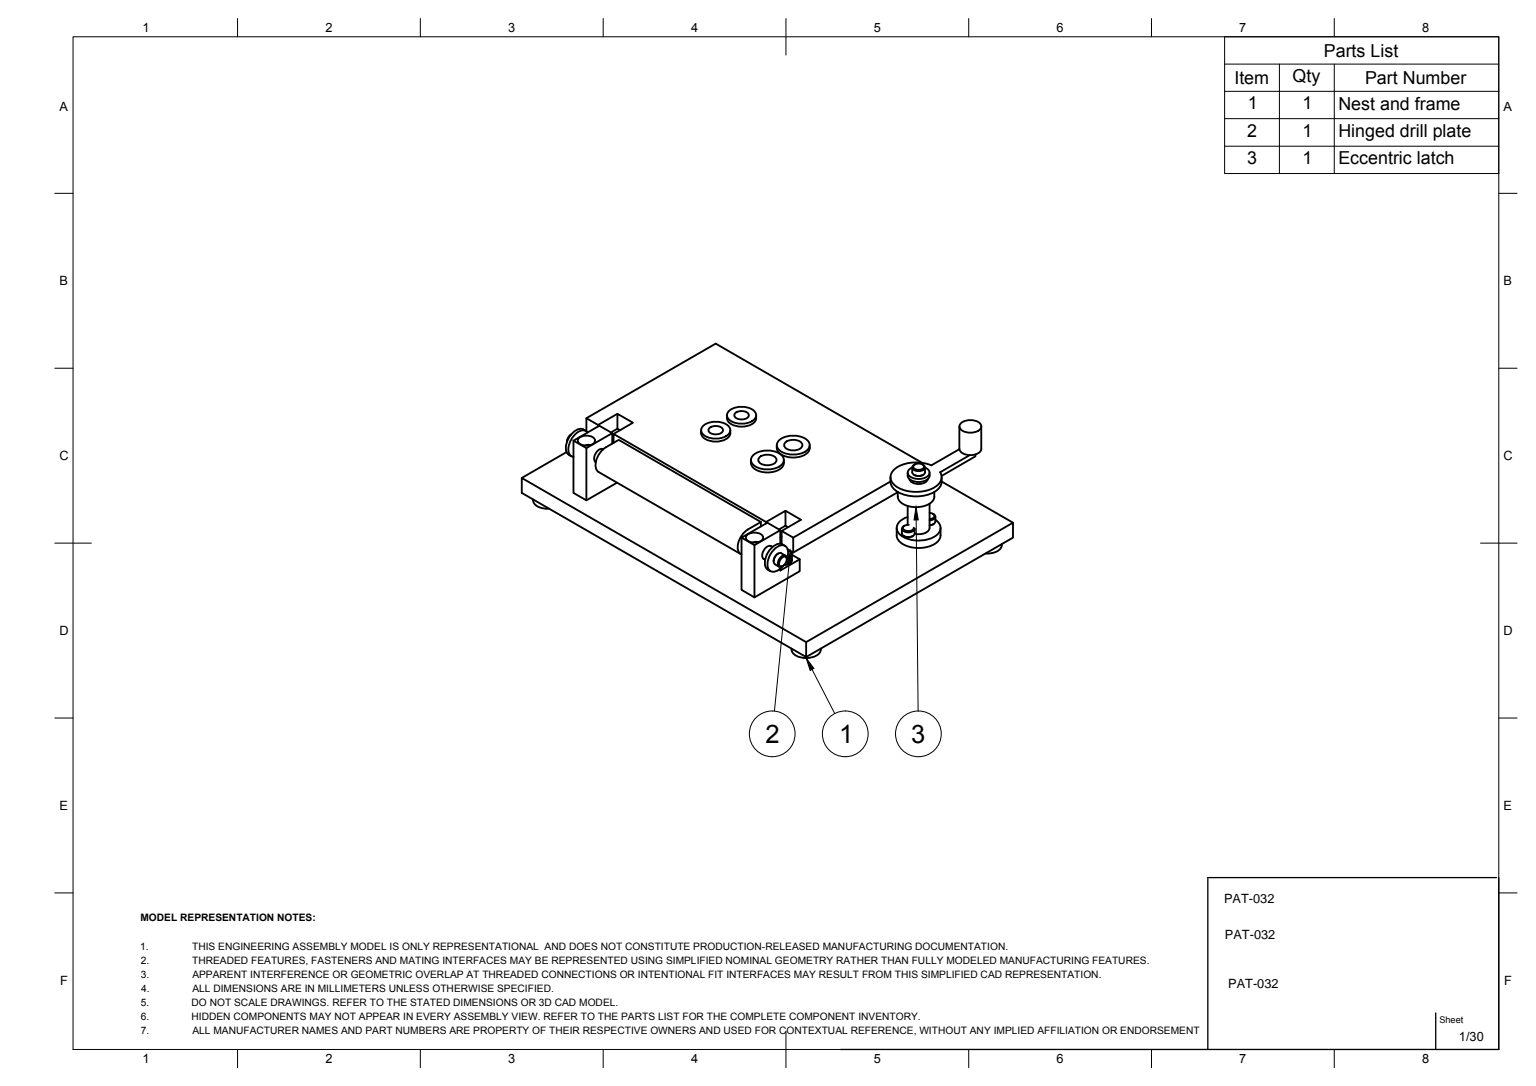
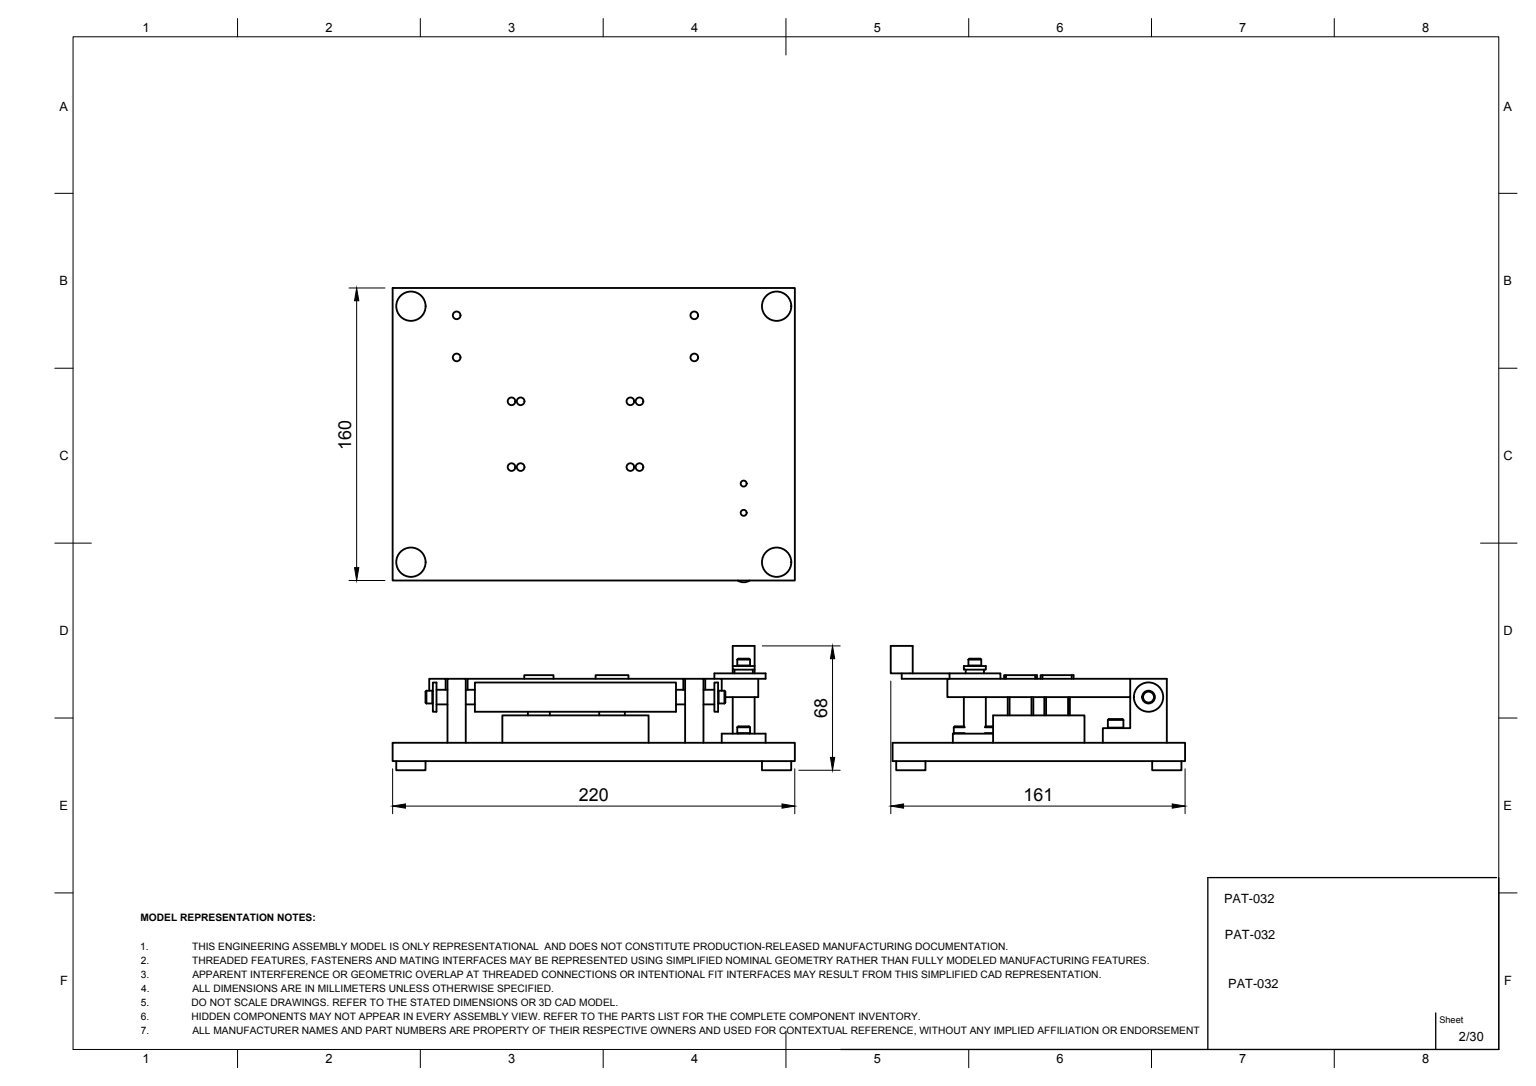
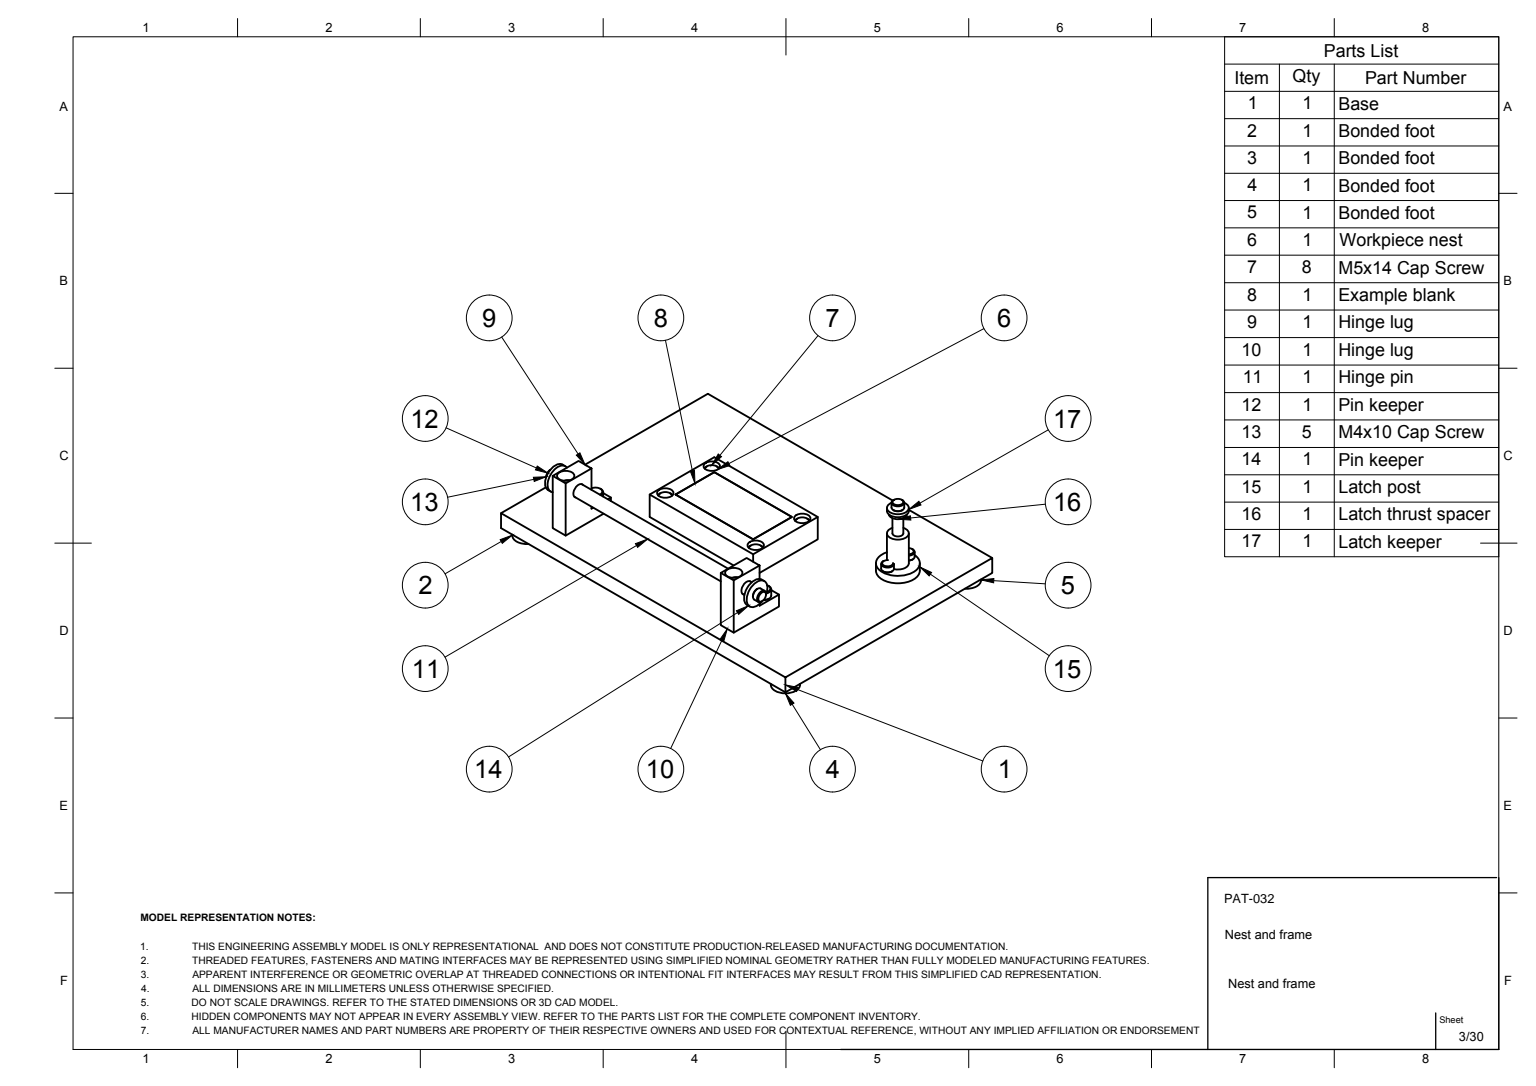
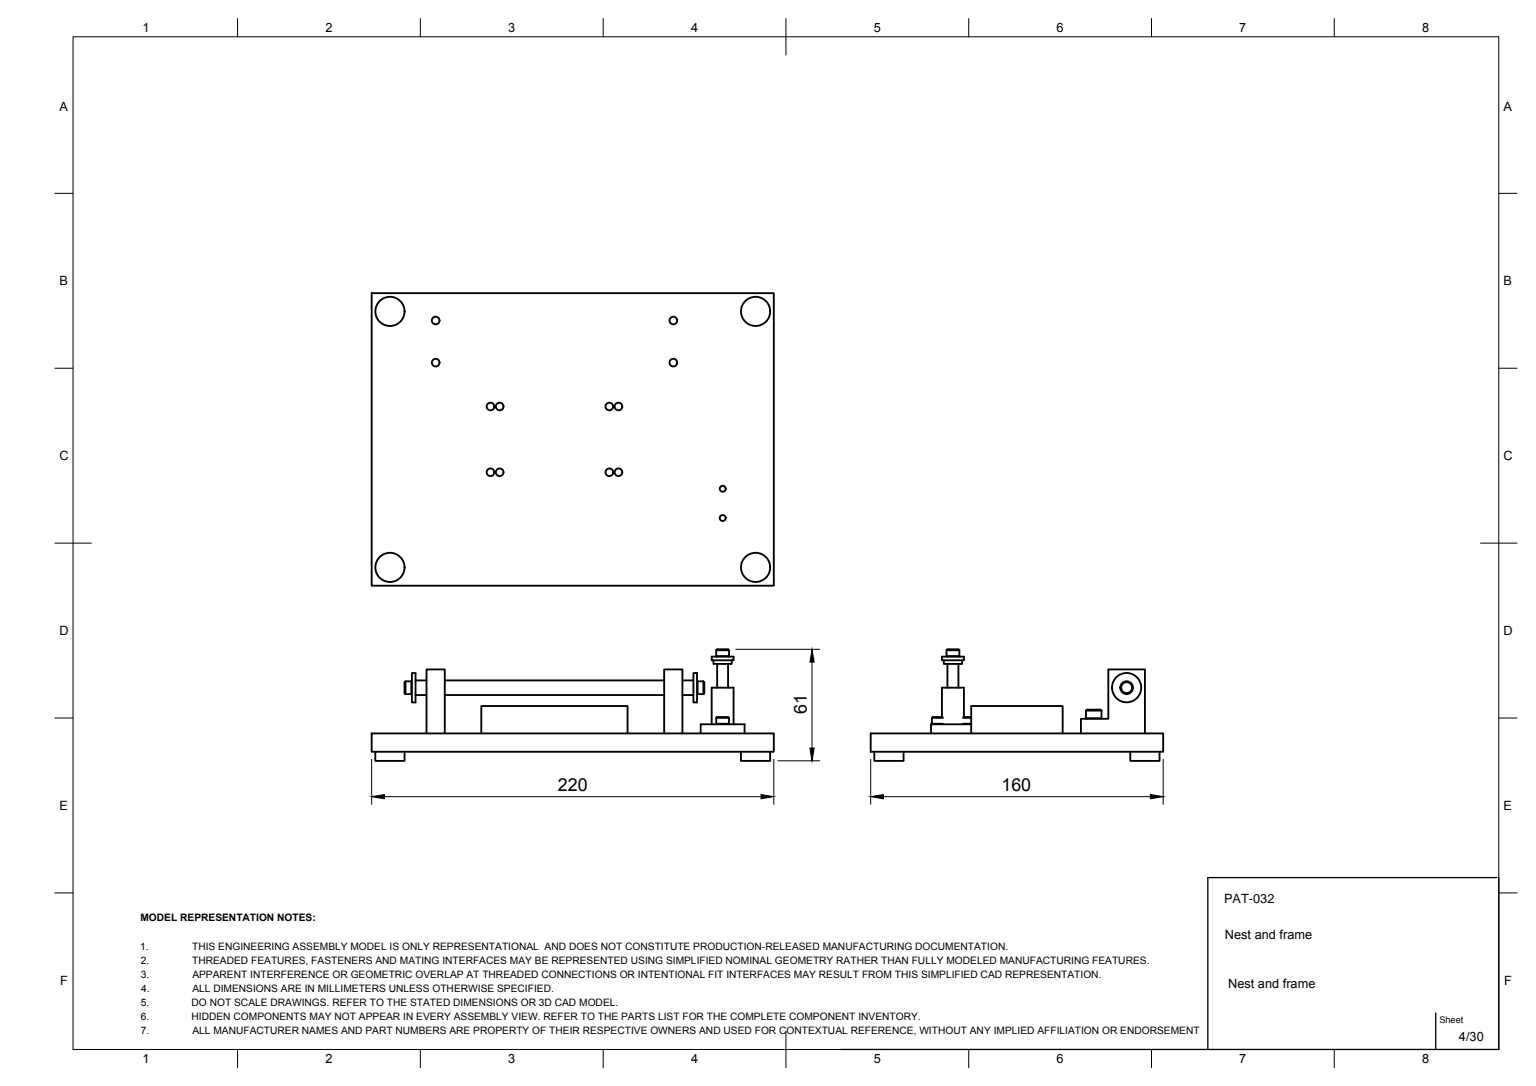
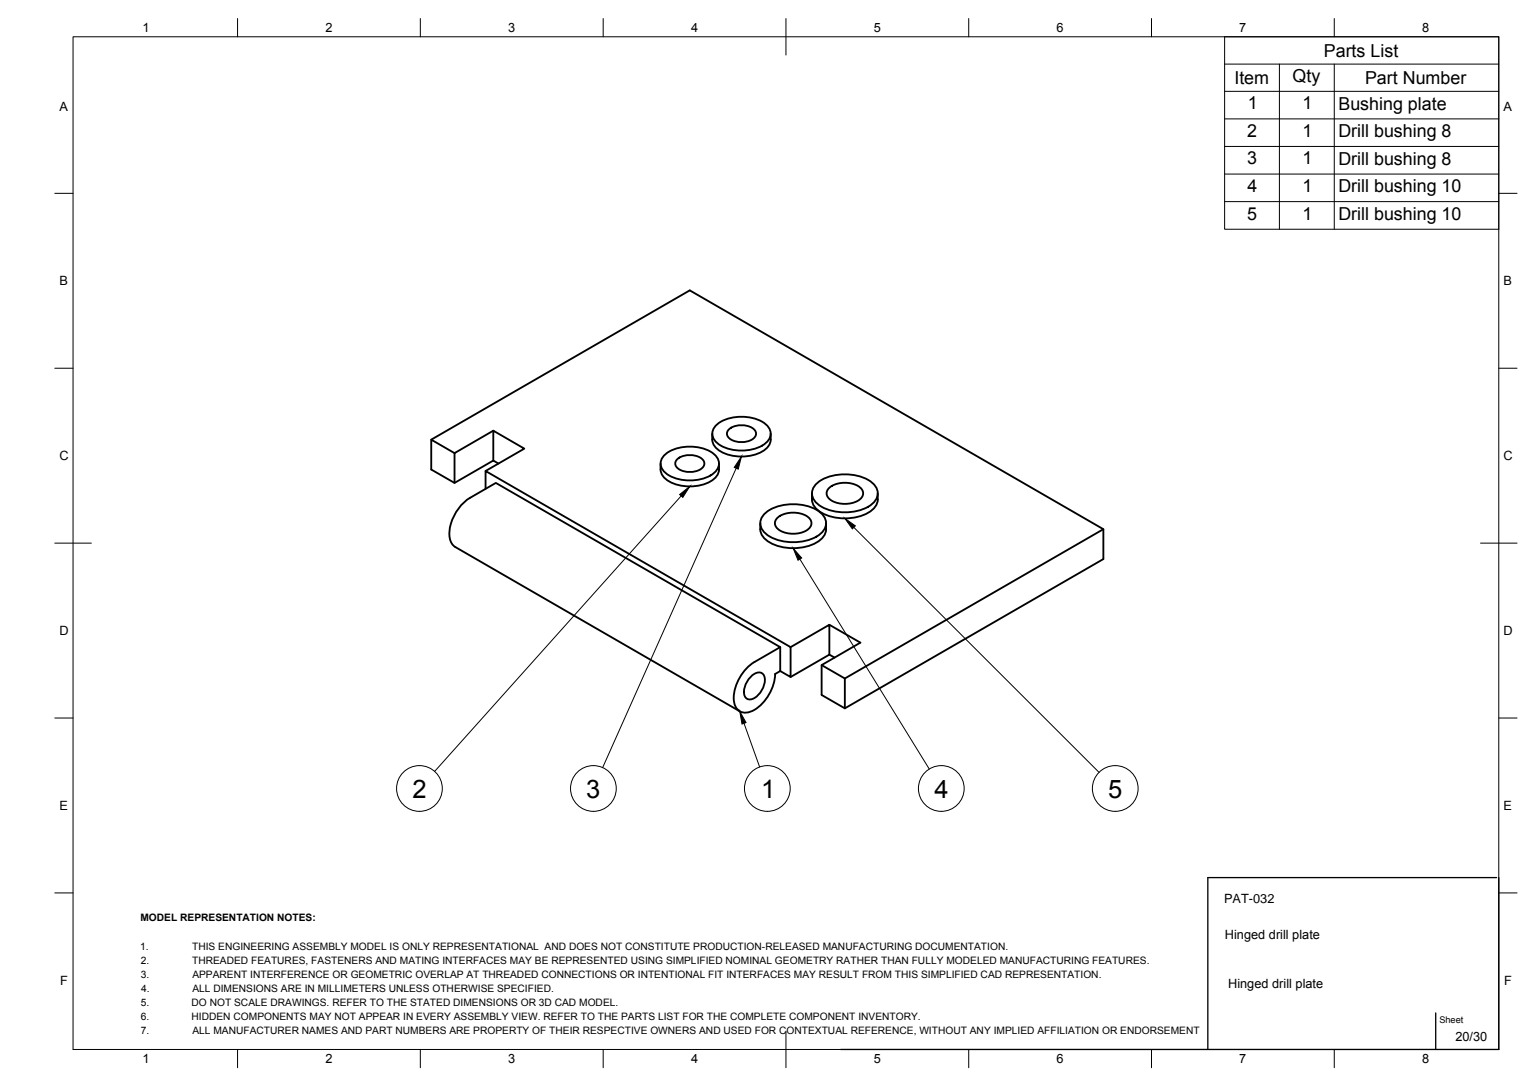
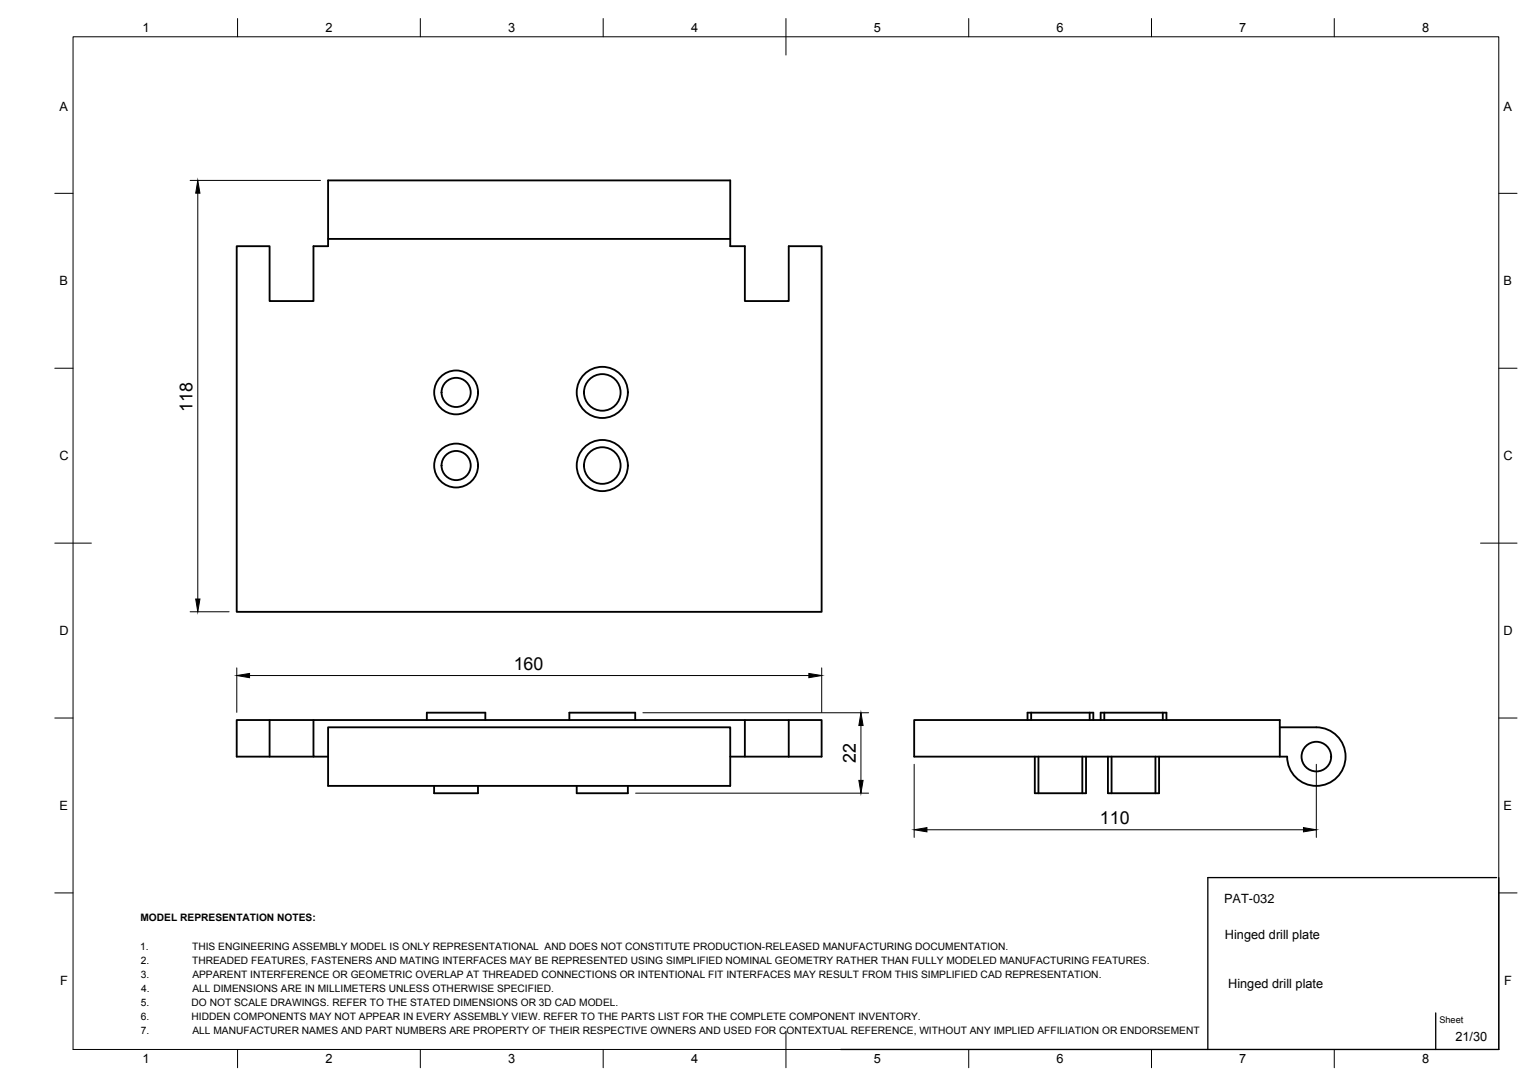
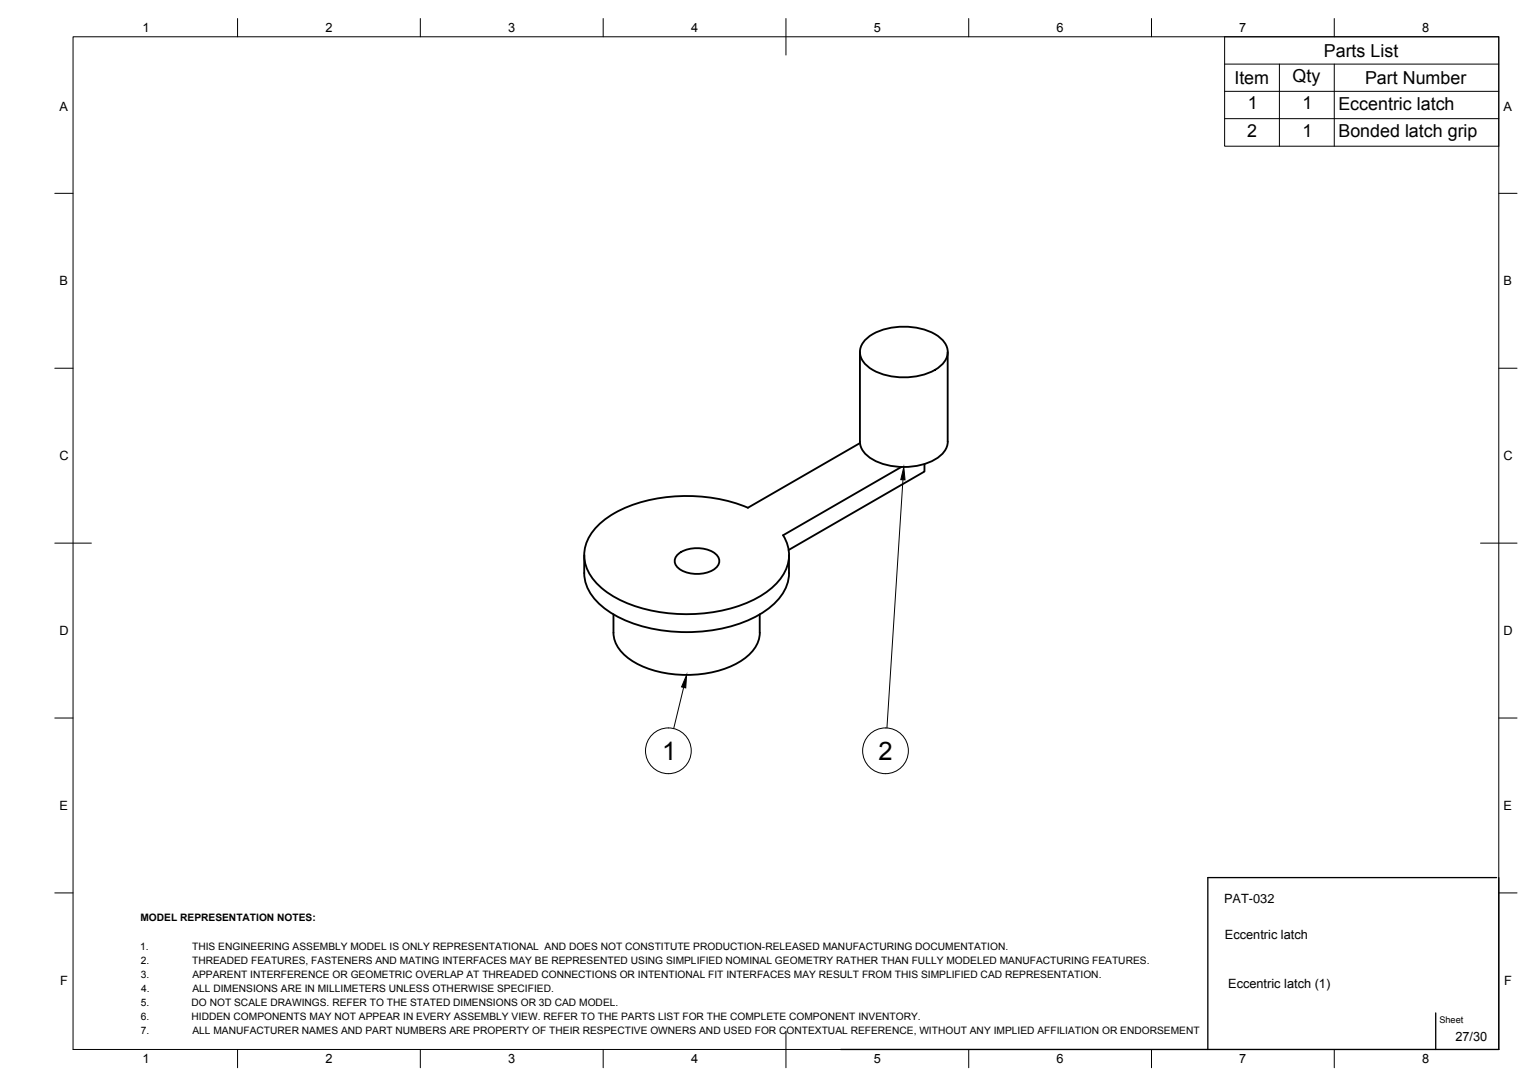
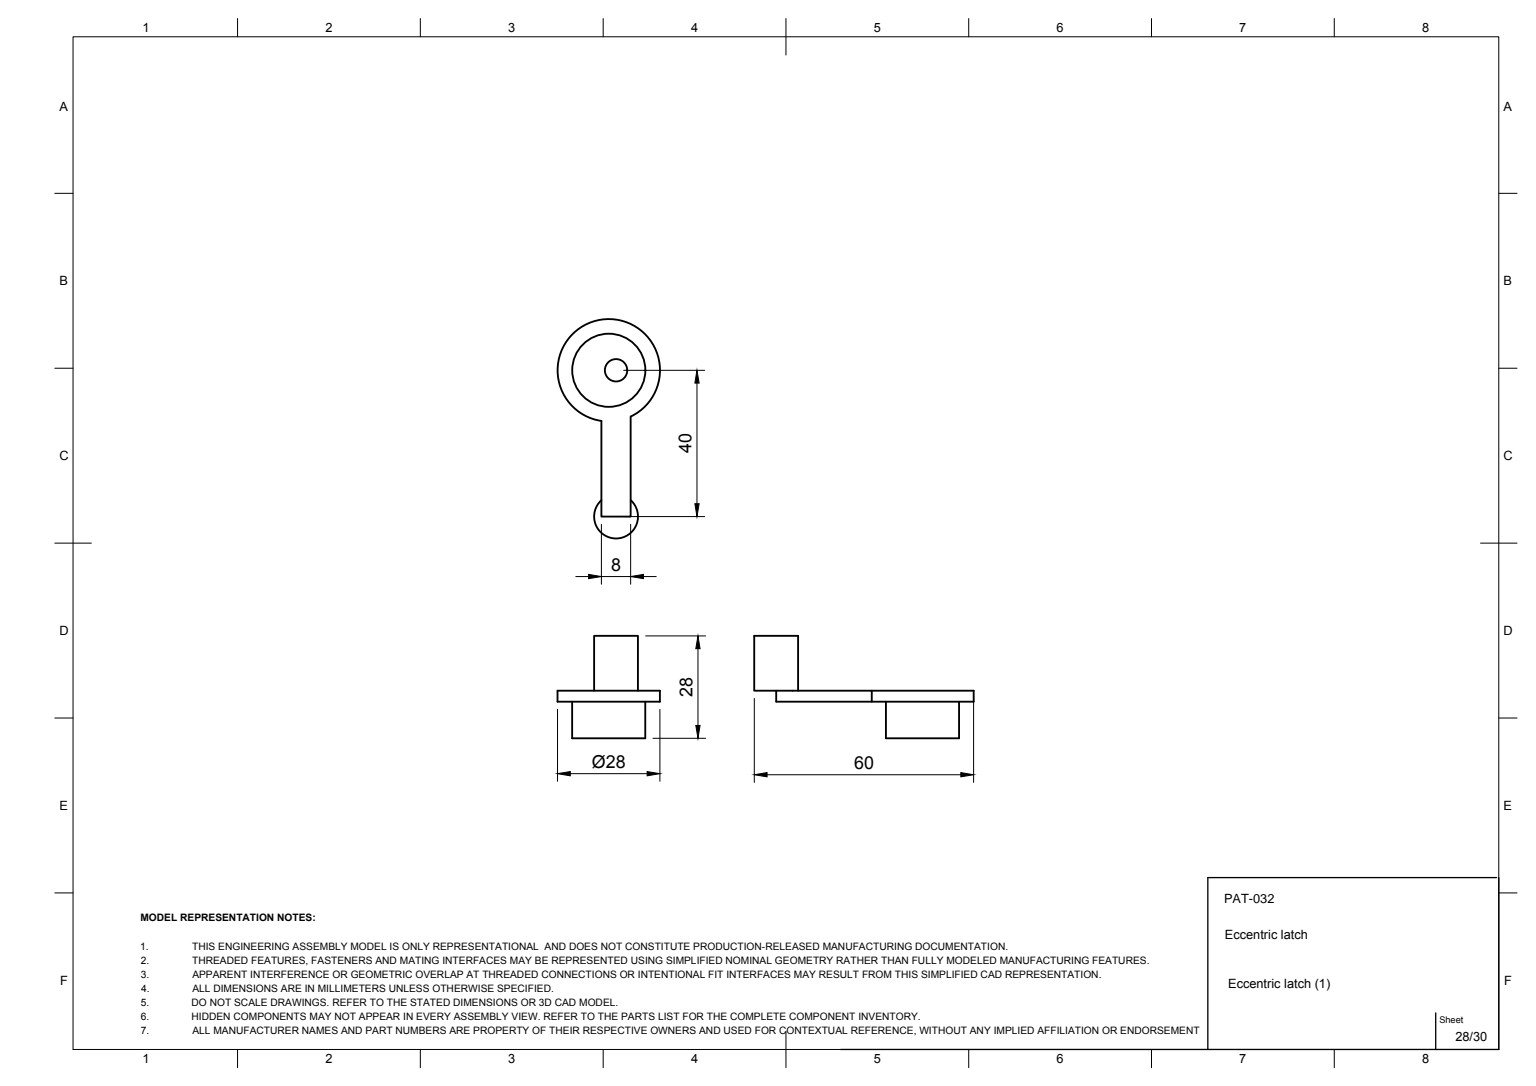
ISO-10303-21;
HEADER;
/* Generated by software containing ST-Developer
 * from STEP Tools, Inc. (www.steptools.com) 
 */

FILE_DESCRIPTION(
/* description */ ('Drill jig with bushing plate'),
/* implementation_level */ '2;1');

FILE_NAME(
/* name */ 'PAT-032',
/* time_stamp */ '2026-10-27T10:51:08-07:00',
/* author */ (''),
/* organization */ (''),
/* preprocessor_version */ 'ST-DEVELOPER v20.2',
/* originating_system */ 'Autodesk Translation Framework v15.17.0.0',
/* authorisation */ '');

FILE_SCHEMA (('AUTOMOTIVE_DESIGN { 1 0 10303 214 3 1 1 }'));
ENDSEC;

DATA;
#10=MECHANICAL_DESIGN_GEOMETRIC_PRESENTATION_REPRESENTATION('',(#223,#224,
#225,#226,#227,#228,#229,#230,#231,#232,#233,#234,#235,#236,#237,#238,#239,
#240,#241,#242,#243,#244,#245,#246),#6638);
#11=ITEM_DEFINED_TRANSFORMATION($,$,#3883,#4179);
#12=ITEM_DEFINED_TRANSFORMATION($,$,#3932,#4180);
#13=ITEM_DEFINED_TRANSFORMATION($,$,#3938,#4181);
#14=ITEM_DEFINED_TRANSFORMATION($,$,#3944,#4182);
#15=ITEM_DEFINED_TRANSFORMATION($,$,#3950,#4183);
#16=ITEM_DEFINED_TRANSFORMATION($,$,#3956,#4184);
#17=ITEM_DEFINED_TRANSFORMATION($,$,#3996,#4185);
#18=ITEM_DEFINED_TRANSFORMATION($,$,#4003,#4186);
#19=ITEM_DEFINED_TRANSFORMATION($,$,#4025,#4187);
#20=ITEM_DEFINED_TRANSFORMATION($,$,#4047,#4188);
#21=ITEM_DEFINED_TRANSFORMATION($,$,#4061,#4189);
#22=ITEM_DEFINED_TRANSFORMATION($,$,#4070,#4190);
#23=ITEM_DEFINED_TRANSFORMATION($,$,#4079,#4191);
#24=ITEM_DEFINED_TRANSFORMATION($,$,#4113,#4192);
#25=ITEM_DEFINED_TRANSFORMATION($,$,#4122,#4193);
#26=ITEM_DEFINED_TRANSFORMATION($,$,#4131,#4194);
#27=ITEM_DEFINED_TRANSFORMATION($,$,#4131,#4195);
#28=ITEM_DEFINED_TRANSFORMATION($,$,#4131,#4196);
#29=ITEM_DEFINED_TRANSFORMATION($,$,#4131,#4197);
#30=ITEM_DEFINED_TRANSFORMATION($,$,#4131,#4198);
#31=ITEM_DEFINED_TRANSFORMATION($,$,#4131,#4199);
#32=ITEM_DEFINED_TRANSFORMATION($,$,#4131,#4200);
#33=ITEM_DEFINED_TRANSFORMATION($,$,#4131,#4201);
#34=ITEM_DEFINED_TRANSFORMATION($,$,#4155,#4202);
#35=ITEM_DEFINED_TRANSFORMATION($,$,#4155,#4203);
#36=ITEM_DEFINED_TRANSFORMATION($,$,#4155,#4204);
#37=ITEM_DEFINED_TRANSFORMATION($,$,#4155,#4205);
#38=ITEM_DEFINED_TRANSFORMATION($,$,#4155,#4206);
#39=ITEM_DEFINED_TRANSFORMATION($,$,#4208,#4296);
#40=ITEM_DEFINED_TRANSFORMATION($,$,#4244,#4297);
#41=ITEM_DEFINED_TRANSFORMATION($,$,#4257,#4298);
#42=ITEM_DEFINED_TRANSFORMATION($,$,#4270,#4299);
#43=ITEM_DEFINED_TRANSFORMATION($,$,#4283,#4300);
#44=ITEM_DEFINED_TRANSFORMATION($,$,#4302,#4324);
#45=ITEM_DEFINED_TRANSFORMATION($,$,#4318,#4325);
#46=ITEM_DEFINED_TRANSFORMATION($,$,#3882,#4326);
#47=ITEM_DEFINED_TRANSFORMATION($,$,#4207,#4327);
#48=ITEM_DEFINED_TRANSFORMATION($,$,#4301,#4328);
#49=(
REPRESENTATION_RELATIONSHIP($,$,#6739,#6738)
REPRESENTATION_RELATIONSHIP_WITH_TRANSFORMATION(#11)
SHAPE_REPRESENTATION_RELATIONSHIP()
);
#50=(
REPRESENTATION_RELATIONSHIP($,$,#6740,#6738)
REPRESENTATION_RELATIONSHIP_WITH_TRANSFORMATION(#12)
SHAPE_REPRESENTATION_RELATIONSHIP()
);
#51=(
REPRESENTATION_RELATIONSHIP($,$,#6741,#6738)
REPRESENTATION_RELATIONSHIP_WITH_TRANSFORMATION(#13)
SHAPE_REPRESENTATION_RELATIONSHIP()
);
#52=(
REPRESENTATION_RELATIONSHIP($,$,#6742,#6738)
REPRESENTATION_RELATIONSHIP_WITH_TRANSFORMATION(#14)
SHAPE_REPRESENTATION_RELATIONSHIP()
);
#53=(
REPRESENTATION_RELATIONSHIP($,$,#6743,#6738)
REPRESENTATION_RELATIONSHIP_WITH_TRANSFORMATION(#15)
SHAPE_REPRESENTATION_RELATIONSHIP()
);
#54=(
REPRESENTATION_RELATIONSHIP($,$,#6744,#6738)
REPRESENTATION_RELATIONSHIP_WITH_TRANSFORMATION(#16)
SHAPE_REPRESENTATION_RELATIONSHIP()
);
#55=(
REPRESENTATION_RELATIONSHIP($,$,#6745,#6738)
REPRESENTATION_RELATIONSHIP_WITH_TRANSFORMATION(#17)
SHAPE_REPRESENTATION_RELATIONSHIP()
);
#56=(
REPRESENTATION_RELATIONSHIP($,$,#6746,#6738)
REPRESENTATION_RELATIONSHIP_WITH_TRANSFORMATION(#18)
SHAPE_REPRESENTATION_RELATIONSHIP()
);
#57=(
REPRESENTATION_RELATIONSHIP($,$,#6747,#6738)
REPRESENTATION_RELATIONSHIP_WITH_TRANSFORMATION(#19)
SHAPE_REPRESENTATION_RELATIONSHIP()
);
#58=(
REPRESENTATION_RELATIONSHIP($,$,#6748,#6738)
REPRESENTATION_RELATIONSHIP_WITH_TRANSFORMATION(#20)
SHAPE_REPRESENTATION_RELATIONSHIP()
);
#59=(
REPRESENTATION_RELATIONSHIP($,$,#6749,#6738)
REPRESENTATION_RELATIONSHIP_WITH_TRANSFORMATION(#21)
SHAPE_REPRESENTATION_RELATIONSHIP()
);
#60=(
REPRESENTATION_RELATIONSHIP($,$,#6750,#6738)
REPRESENTATION_RELATIONSHIP_WITH_TRANSFORMATION(#22)
SHAPE_REPRESENTATION_RELATIONSHIP()
);
#61=(
REPRESENTATION_RELATIONSHIP($,$,#6751,#6738)
REPRESENTATION_RELATIONSHIP_WITH_TRANSFORMATION(#23)
SHAPE_REPRESENTATION_RELATIONSHIP()
);
#62=(
REPRESENTATION_RELATIONSHIP($,$,#6752,#6738)
REPRESENTATION_RELATIONSHIP_WITH_TRANSFORMATION(#24)
SHAPE_REPRESENTATION_RELATIONSHIP()
);
#63=(
REPRESENTATION_RELATIONSHIP($,$,#6753,#6738)
REPRESENTATION_RELATIONSHIP_WITH_TRANSFORMATION(#25)
SHAPE_REPRESENTATION_RELATIONSHIP()
);
#64=(
REPRESENTATION_RELATIONSHIP($,$,#6754,#6738)
REPRESENTATION_RELATIONSHIP_WITH_TRANSFORMATION(#26)
SHAPE_REPRESENTATION_RELATIONSHIP()
);
#65=(
REPRESENTATION_RELATIONSHIP($,$,#6754,#6738)
REPRESENTATION_RELATIONSHIP_WITH_TRANSFORMATION(#27)
SHAPE_REPRESENTATION_RELATIONSHIP()
);
#66=(
REPRESENTATION_RELATIONSHIP($,$,#6754,#6738)
REPRESENTATION_RELATIONSHIP_WITH_TRANSFORMATION(#28)
SHAPE_REPRESENTATION_RELATIONSHIP()
);
#67=(
REPRESENTATION_RELATIONSHIP($,$,#6754,#6738)
REPRESENTATION_RELATIONSHIP_WITH_TRANSFORMATION(#29)
SHAPE_REPRESENTATION_RELATIONSHIP()
);
#68=(
REPRESENTATION_RELATIONSHIP($,$,#6754,#6738)
REPRESENTATION_RELATIONSHIP_WITH_TRANSFORMATION(#30)
SHAPE_REPRESENTATION_RELATIONSHIP()
);
#69=(
REPRESENTATION_RELATIONSHIP($,$,#6754,#6738)
REPRESENTATION_RELATIONSHIP_WITH_TRANSFORMATION(#31)
SHAPE_REPRESENTATION_RELATIONSHIP()
);
#70=(
REPRESENTATION_RELATIONSHIP($,$,#6754,#6738)
REPRESENTATION_RELATIONSHIP_WITH_TRANSFORMATION(#32)
SHAPE_REPRESENTATION_RELATIONSHIP()
);
#71=(
REPRESENTATION_RELATIONSHIP($,$,#6754,#6738)
REPRESENTATION_RELATIONSHIP_WITH_TRANSFORMATION(#33)
SHAPE_REPRESENTATION_RELATIONSHIP()
);
#72=(
REPRESENTATION_RELATIONSHIP($,$,#6755,#6738)
REPRESENTATION_RELATIONSHIP_WITH_TRANSFORMATION(#34)
SHAPE_REPRESENTATION_RELATIONSHIP()
);
#73=(
REPRESENTATION_RELATIONSHIP($,$,#6755,#6738)
REPRESENTATION_RELATIONSHIP_WITH_TRANSFORMATION(#35)
SHAPE_REPRESENTATION_RELATIONSHIP()
);
#74=(
REPRESENTATION_RELATIONSHIP($,$,#6755,#6738)
REPRESENTATION_RELATIONSHIP_WITH_TRANSFORMATION(#36)
SHAPE_REPRESENTATION_RELATIONSHIP()
);
#75=(
REPRESENTATION_RELATIONSHIP($,$,#6755,#6738)
REPRESENTATION_RELATIONSHIP_WITH_TRANSFORMATION(#37)
SHAPE_REPRESENTATION_RELATIONSHIP()
);
#76=(
REPRESENTATION_RELATIONSHIP($,$,#6755,#6738)
REPRESENTATION_RELATIONSHIP_WITH_TRANSFORMATION(#38)
SHAPE_REPRESENTATION_RELATIONSHIP()
);
#77=(
REPRESENTATION_RELATIONSHIP($,$,#6757,#6756)
REPRESENTATION_RELATIONSHIP_WITH_TRANSFORMATION(#39)
SHAPE_REPRESENTATION_RELATIONSHIP()
);
#78=(
REPRESENTATION_RELATIONSHIP($,$,#6758,#6756)
REPRESENTATION_RELATIONSHIP_WITH_TRANSFORMATION(#40)
SHAPE_REPRESENTATION_RELATIONSHIP()
);
#79=(
REPRESENTATION_RELATIONSHIP($,$,#6759,#6756)
REPRESENTATION_RELATIONSHIP_WITH_TRANSFORMATION(#41)
SHAPE_REPRESENTATION_RELATIONSHIP()
);
#80=(
REPRESENTATION_RELATIONSHIP($,$,#6760,#6756)
REPRESENTATION_RELATIONSHIP_WITH_TRANSFORMATION(#42)
SHAPE_REPRESENTATION_RELATIONSHIP()
);
#81=(
REPRESENTATION_RELATIONSHIP($,$,#6761,#6756)
REPRESENTATION_RELATIONSHIP_WITH_TRANSFORMATION(#43)
SHAPE_REPRESENTATION_RELATIONSHIP()
);
#82=(
REPRESENTATION_RELATIONSHIP($,$,#6763,#6762)
REPRESENTATION_RELATIONSHIP_WITH_TRANSFORMATION(#44)
SHAPE_REPRESENTATION_RELATIONSHIP()
);
#83=(
REPRESENTATION_RELATIONSHIP($,$,#6764,#6762)
REPRESENTATION_RELATIONSHIP_WITH_TRANSFORMATION(#45)
SHAPE_REPRESENTATION_RELATIONSHIP()
);
#84=(
REPRESENTATION_RELATIONSHIP($,$,#6738,#6737)
REPRESENTATION_RELATIONSHIP_WITH_TRANSFORMATION(#46)
SHAPE_REPRESENTATION_RELATIONSHIP()
);
#85=(
REPRESENTATION_RELATIONSHIP($,$,#6756,#6737)
REPRESENTATION_RELATIONSHIP_WITH_TRANSFORMATION(#47)
SHAPE_REPRESENTATION_RELATIONSHIP()
);
#86=(
REPRESENTATION_RELATIONSHIP($,$,#6762,#6737)
REPRESENTATION_RELATIONSHIP_WITH_TRANSFORMATION(#48)
SHAPE_REPRESENTATION_RELATIONSHIP()
);
#87=CONTEXT_DEPENDENT_SHAPE_REPRESENTATION(#49,#6690);
#88=CONTEXT_DEPENDENT_SHAPE_REPRESENTATION(#50,#6691);
#89=CONTEXT_DEPENDENT_SHAPE_REPRESENTATION(#51,#6692);
#90=CONTEXT_DEPENDENT_SHAPE_REPRESENTATION(#52,#6693);
#91=CONTEXT_DEPENDENT_SHAPE_REPRESENTATION(#53,#6694);
#92=CONTEXT_DEPENDENT_SHAPE_REPRESENTATION(#54,#6695);
#93=CONTEXT_DEPENDENT_SHAPE_REPRESENTATION(#55,#6696);
#94=CONTEXT_DEPENDENT_SHAPE_REPRESENTATION(#56,#6697);
#95=CONTEXT_DEPENDENT_SHAPE_REPRESENTATION(#57,#6698);
#96=CONTEXT_DEPENDENT_SHAPE_REPRESENTATION(#58,#6699);
#97=CONTEXT_DEPENDENT_SHAPE_REPRESENTATION(#59,#6700);
#98=CONTEXT_DEPENDENT_SHAPE_REPRESENTATION(#60,#6701);
#99=CONTEXT_DEPENDENT_SHAPE_REPRESENTATION(#61,#6702);
#100=CONTEXT_DEPENDENT_SHAPE_REPRESENTATION(#62,#6703);
#101=CONTEXT_DEPENDENT_SHAPE_REPRESENTATION(#63,#6704);
#102=CONTEXT_DEPENDENT_SHAPE_REPRESENTATION(#64,#6705);
#103=CONTEXT_DEPENDENT_SHAPE_REPRESENTATION(#65,#6706);
#104=CONTEXT_DEPENDENT_SHAPE_REPRESENTATION(#66,#6707);
#105=CONTEXT_DEPENDENT_SHAPE_REPRESENTATION(#67,#6708);
#106=CONTEXT_DEPENDENT_SHAPE_REPRESENTATION(#68,#6709);
#107=CONTEXT_DEPENDENT_SHAPE_REPRESENTATION(#69,#6710);
#108=CONTEXT_DEPENDENT_SHAPE_REPRESENTATION(#70,#6711);
#109=CONTEXT_DEPENDENT_SHAPE_REPRESENTATION(#71,#6712);
#110=CONTEXT_DEPENDENT_SHAPE_REPRESENTATION(#72,#6713);
#111=CONTEXT_DEPENDENT_SHAPE_REPRESENTATION(#73,#6714);
#112=CONTEXT_DEPENDENT_SHAPE_REPRESENTATION(#74,#6715);
#113=CONTEXT_DEPENDENT_SHAPE_REPRESENTATION(#75,#6716);
#114=CONTEXT_DEPENDENT_SHAPE_REPRESENTATION(#76,#6717);
#115=CONTEXT_DEPENDENT_SHAPE_REPRESENTATION(#77,#6724);
#116=CONTEXT_DEPENDENT_SHAPE_REPRESENTATION(#78,#6725);
#117=CONTEXT_DEPENDENT_SHAPE_REPRESENTATION(#79,#6726);
#118=CONTEXT_DEPENDENT_SHAPE_REPRESENTATION(#80,#6727);
#119=CONTEXT_DEPENDENT_SHAPE_REPRESENTATION(#81,#6728);
#120=CONTEXT_DEPENDENT_SHAPE_REPRESENTATION(#82,#6732);
#121=CONTEXT_DEPENDENT_SHAPE_REPRESENTATION(#83,#6733);
#122=CONTEXT_DEPENDENT_SHAPE_REPRESENTATION(#84,#6734);
#123=CONTEXT_DEPENDENT_SHAPE_REPRESENTATION(#85,#6735);
#124=CONTEXT_DEPENDENT_SHAPE_REPRESENTATION(#86,#6736);
#125=NEXT_ASSEMBLY_USAGE_OCCURRENCE('Base:1','Base:1','Base:1',#6767,#6768,
'Base:1');
#126=NEXT_ASSEMBLY_USAGE_OCCURRENCE('Bonded foot:1','Bonded foot:1',
'Bonded foot:1',#6767,#6769,'Bonded foot:1');
#127=NEXT_ASSEMBLY_USAGE_OCCURRENCE('Bonded foot (1):1',
'Bonded foot (1):1','Bonded foot (1):1',#6767,#6770,'Bonded foot (1):1');
#128=NEXT_ASSEMBLY_USAGE_OCCURRENCE('Bonded foot (2):1',
'Bonded foot (2):1','Bonded foot (2):1',#6767,#6771,'Bonded foot (2):1');
#129=NEXT_ASSEMBLY_USAGE_OCCURRENCE('Bonded foot (3):1',
'Bonded foot (3):1','Bonded foot (3):1',#6767,#6772,'Bonded foot (3):1');
#130=NEXT_ASSEMBLY_USAGE_OCCURRENCE('Workpiece nest:1',
'Workpiece nest:1','Workpiece nest:1',#6767,#6773,'Workpiece nest:1');
#131=NEXT_ASSEMBLY_USAGE_OCCURRENCE('Example blank:1','Example blank:1',
'Example blank:1',#6767,#6774,'Example blank:1');
#132=NEXT_ASSEMBLY_USAGE_OCCURRENCE('Hinge lug:1','Hinge lug:1',
'Hinge lug:1',#6767,#6775,'Hinge lug:1');
#133=NEXT_ASSEMBLY_USAGE_OCCURRENCE('Hinge lug (1):1','Hinge lug (1):1',
'Hinge lug (1):1',#6767,#6776,'Hinge lug (1):1');
#134=NEXT_ASSEMBLY_USAGE_OCCURRENCE('Hinge pin:1','Hinge pin:1',
'Hinge pin:1',#6767,#6777,'Hinge pin:1');
#135=NEXT_ASSEMBLY_USAGE_OCCURRENCE('Pin keeper:1','Pin keeper:1',
'Pin keeper:1',#6767,#6778,'Pin keeper:1');
#136=NEXT_ASSEMBLY_USAGE_OCCURRENCE('Pin keeper (1):1',
'Pin keeper (1):1','Pin keeper (1):1',#6767,#6779,'Pin keeper (1):1');
#137=NEXT_ASSEMBLY_USAGE_OCCURRENCE('Latch post:1','Latch post:1',
'Latch post:1',#6767,#6780,'Latch post:1');
#138=NEXT_ASSEMBLY_USAGE_OCCURRENCE('Latch thrust spacer:1',
'Latch thrust spacer:1','Latch thrust spacer:1',#6767,#6781,
'Latch thrust spacer:1');
#139=NEXT_ASSEMBLY_USAGE_OCCURRENCE('Latch keeper:1','Latch keeper:1',
'Latch keeper:1',#6767,#6782,'Latch keeper:1');
#140=NEXT_ASSEMBLY_USAGE_OCCURRENCE('M5x14 Cap Screw:2',
'M5x14 Cap Screw:2','M5x14 Cap Screw:2',#6767,#6783,'M5x14 Cap Screw:2');
#141=NEXT_ASSEMBLY_USAGE_OCCURRENCE('M5x14 Cap Screw:3',
'M5x14 Cap Screw:3','M5x14 Cap Screw:3',#6767,#6783,'M5x14 Cap Screw:3');
#142=NEXT_ASSEMBLY_USAGE_OCCURRENCE('M5x14 Cap Screw:4',
'M5x14 Cap Screw:4','M5x14 Cap Screw:4',#6767,#6783,'M5x14 Cap Screw:4');
#143=NEXT_ASSEMBLY_USAGE_OCCURRENCE('M5x14 Cap Screw:5',
'M5x14 Cap Screw:5','M5x14 Cap Screw:5',#6767,#6783,'M5x14 Cap Screw:5');
#144=NEXT_ASSEMBLY_USAGE_OCCURRENCE('M5x14 Cap Screw:6',
'M5x14 Cap Screw:6','M5x14 Cap Screw:6',#6767,#6783,'M5x14 Cap Screw:6');
#145=NEXT_ASSEMBLY_USAGE_OCCURRENCE('M5x14 Cap Screw:7',
'M5x14 Cap Screw:7','M5x14 Cap Screw:7',#6767,#6783,'M5x14 Cap Screw:7');
#146=NEXT_ASSEMBLY_USAGE_OCCURRENCE('M5x14 Cap Screw:8',
'M5x14 Cap Screw:8','M5x14 Cap Screw:8',#6767,#6783,'M5x14 Cap Screw:8');
#147=NEXT_ASSEMBLY_USAGE_OCCURRENCE('M5x14 Cap Screw:9',
'M5x14 Cap Screw:9','M5x14 Cap Screw:9',#6767,#6783,'M5x14 Cap Screw:9');
#148=NEXT_ASSEMBLY_USAGE_OCCURRENCE('M4x10 Cap Screw:2',
'M4x10 Cap Screw:2','M4x10 Cap Screw:2',#6767,#6784,'M4x10 Cap Screw:2');
#149=NEXT_ASSEMBLY_USAGE_OCCURRENCE('M4x10 Cap Screw:3',
'M4x10 Cap Screw:3','M4x10 Cap Screw:3',#6767,#6784,'M4x10 Cap Screw:3');
#150=NEXT_ASSEMBLY_USAGE_OCCURRENCE('M4x10 Cap Screw:4',
'M4x10 Cap Screw:4','M4x10 Cap Screw:4',#6767,#6784,'M4x10 Cap Screw:4');
#151=NEXT_ASSEMBLY_USAGE_OCCURRENCE('M4x10 Cap Screw:5',
'M4x10 Cap Screw:5','M4x10 Cap Screw:5',#6767,#6784,'M4x10 Cap Screw:5');
#152=NEXT_ASSEMBLY_USAGE_OCCURRENCE('M4x10 Cap Screw:6',
'M4x10 Cap Screw:6','M4x10 Cap Screw:6',#6767,#6784,'M4x10 Cap Screw:6');
#153=NEXT_ASSEMBLY_USAGE_OCCURRENCE('Bushing plate:1','Bushing plate:1',
'Bushing plate:1',#6785,#6786,'Bushing plate:1');
#154=NEXT_ASSEMBLY_USAGE_OCCURRENCE('Drill bushing 8:1',
'Drill bushing 8:1','Drill bushing 8:1',#6785,#6787,'Drill bushing 8:1');
#155=NEXT_ASSEMBLY_USAGE_OCCURRENCE('Drill bushing 8 (1):1',
'Drill bushing 8 (1):1','Drill bushing 8 (1):1',#6785,#6788,
'Drill bushing 8 (1):1');
#156=NEXT_ASSEMBLY_USAGE_OCCURRENCE('Drill bushing 10:1',
'Drill bushing 10:1','Drill bushing 10:1',#6785,#6789,
'Drill bushing 10:1');
#157=NEXT_ASSEMBLY_USAGE_OCCURRENCE('Drill bushing 10 (1):1',
'Drill bushing 10 (1):1','Drill bushing 10 (1):1',#6785,#6790,
'Drill bushing 10 (1):1');
#158=NEXT_ASSEMBLY_USAGE_OCCURRENCE('Eccentric latch:1',
'Eccentric latch:1','Eccentric latch:1',#6791,#6792,'Eccentric latch:1');
#159=NEXT_ASSEMBLY_USAGE_OCCURRENCE('Bonded latch grip:1',
'Bonded latch grip:1','Bonded latch grip:1',#6791,#6793,
'Bonded latch grip:1');
#160=NEXT_ASSEMBLY_USAGE_OCCURRENCE('Nest and frame:1',
'Nest and frame:1','Nest and frame:1',#6766,#6767,'Nest and frame:1');
#161=NEXT_ASSEMBLY_USAGE_OCCURRENCE('Hinged drill plate:1',
'Hinged drill plate:1','Hinged drill plate:1',#6766,#6785,
'Hinged drill plate:1');
#162=NEXT_ASSEMBLY_USAGE_OCCURRENCE('Eccentric latch (1):1',
'Eccentric latch (1):1','Eccentric latch (1):1',#6766,#6791,
'Eccentric latch (1):1');
#163=CONICAL_SURFACE('',#4144,0.4,0.785398163397448);
#164=CONICAL_SURFACE('',#4148,0.41,0.785398163397448);
#165=CONICAL_SURFACE('',#4152,0.26,0.463647609000806);
#166=CONICAL_SURFACE('',#4168,0.325,0.785398163397448);
#167=CONICAL_SURFACE('',#4172,0.335,0.785398163397448);
#168=CONICAL_SURFACE('',#4176,0.21,0.463647609000806);
#169=ORIENTED_CLOSED_SHELL('',*,#3605,.F.);
#170=ORIENTED_CLOSED_SHELL('',*,#3607,.F.);
#171=BREP_WITH_VOIDS('Body1',#3606,(#169));
#172=BREP_WITH_VOIDS('Body1',#3608,(#170));
#173=B_SPLINE_CURVE_WITH_KNOTS('',3,(#5774,#5775,#5776,#5777,#5778,#5779,
#5780,#5781,#5782,#5783,#5784,#5785,#5786,#5787,#5788,#5789,#5790,#5791,
#5792,#5793,#5794,#5795,#5796,#5797,#5798,#5799,#5800,#5801,#5802,#5803,
#5804,#5805,#5806,#5807,#5808,#5809,#5810,#5811,#5812,#5813,#5814,#5815,
#5816,#5817,#5818,#5819,#5820,#5821,#5822,#5823),.UNSPECIFIED.,.T.,.F.,
(4,2,2,2,2,2,2,2,2,2,2,2,2,2,2,2,2,2,2,2,2,2,2,2,4),(0.,0.177519856988816,
0.355039713977633,0.436196019741432,0.517352325505232,0.678532215702782,
0.839712105900332,1.00089199609788,1.16207188629543,1.24322819205923,1.32438449782303,
1.50190435481185,1.67942421180066,1.85694406878948,2.0344639257783,2.1156202315421,
2.1967765373059,2.35795642750345,2.519136317701,2.68031620789855,2.8414960980961,
2.9226524038599,3.0038087096237,3.18132856661251,3.35884842360133),
 .UNSPECIFIED.);
#174=B_SPLINE_CURVE_WITH_KNOTS('',3,(#5889,#5890,#5891,#5892,#5893,#5894,
#5895,#5896,#5897,#5898,#5899,#5900,#5901,#5902,#5903,#5904,#5905,#5906,
#5907,#5908,#5909,#5910,#5911,#5912,#5913,#5914,#5915,#5916,#5917,#5918,
#5919,#5920,#5921,#5922,#5923,#5924,#5925,#5926,#5927,#5928,#5929,#5930,
#5931,#5932,#5933,#5934,#5935,#5936,#5937,#5938),.UNSPECIFIED.,.T.,.F.,
(4,2,2,2,2,2,2,2,2,2,2,2,2,2,2,2,2,2,2,2,2,2,2,2,4),(0.,0.177519856988816,
0.355039713977633,0.436196019741432,0.517352325505232,0.678532215702782,
0.839712105900332,1.00089199609788,1.16207188629543,1.24322819205923,1.32438449782303,
1.50190435481185,1.67942421180066,1.85694406878948,2.0344639257783,2.1156202315421,
2.1967765373059,2.35795642750345,2.519136317701,2.68031620789855,2.8414960980961,
2.9226524038599,3.0038087096237,3.18132856661251,3.35884842360133),
 .UNSPECIFIED.);
#175=SHAPE_REPRESENTATION_RELATIONSHIP('SRR','None',#6739,#199);
#176=SHAPE_REPRESENTATION_RELATIONSHIP('SRR','None',#6740,#200);
#177=SHAPE_REPRESENTATION_RELATIONSHIP('SRR','None',#6741,#201);
#178=SHAPE_REPRESENTATION_RELATIONSHIP('SRR','None',#6742,#202);
#179=SHAPE_REPRESENTATION_RELATIONSHIP('SRR','None',#6743,#203);
#180=SHAPE_REPRESENTATION_RELATIONSHIP('SRR','None',#6744,#204);
#181=SHAPE_REPRESENTATION_RELATIONSHIP('SRR','None',#6745,#205);
#182=SHAPE_REPRESENTATION_RELATIONSHIP('SRR','None',#6746,#206);
#183=SHAPE_REPRESENTATION_RELATIONSHIP('SRR','None',#6747,#207);
#184=SHAPE_REPRESENTATION_RELATIONSHIP('SRR','None',#6748,#208);
#185=SHAPE_REPRESENTATION_RELATIONSHIP('SRR','None',#6749,#209);
#186=SHAPE_REPRESENTATION_RELATIONSHIP('SRR','None',#6750,#210);
#187=SHAPE_REPRESENTATION_RELATIONSHIP('SRR','None',#6751,#211);
#188=SHAPE_REPRESENTATION_RELATIONSHIP('SRR','None',#6752,#212);
#189=SHAPE_REPRESENTATION_RELATIONSHIP('SRR','None',#6753,#213);
#190=SHAPE_REPRESENTATION_RELATIONSHIP('SRR','None',#6754,#214);
#191=SHAPE_REPRESENTATION_RELATIONSHIP('SRR','None',#6755,#215);
#192=SHAPE_REPRESENTATION_RELATIONSHIP('SRR','None',#6757,#216);
#193=SHAPE_REPRESENTATION_RELATIONSHIP('SRR','None',#6758,#217);
#194=SHAPE_REPRESENTATION_RELATIONSHIP('SRR','None',#6759,#218);
#195=SHAPE_REPRESENTATION_RELATIONSHIP('SRR','None',#6760,#219);
#196=SHAPE_REPRESENTATION_RELATIONSHIP('SRR','None',#6761,#220);
#197=SHAPE_REPRESENTATION_RELATIONSHIP('SRR','None',#6763,#221);
#198=SHAPE_REPRESENTATION_RELATIONSHIP('SRR','None',#6764,#222);
#199=ADVANCED_BREP_SHAPE_REPRESENTATION('',(#247),#6612);
#200=ADVANCED_BREP_SHAPE_REPRESENTATION('',(#248),#6613);
#201=ADVANCED_BREP_SHAPE_REPRESENTATION('',(#249),#6614);
#202=ADVANCED_BREP_SHAPE_REPRESENTATION('',(#250),#6615);
#203=ADVANCED_BREP_SHAPE_REPRESENTATION('',(#251),#6616);
#204=ADVANCED_BREP_SHAPE_REPRESENTATION('',(#252),#6617);
#205=ADVANCED_BREP_SHAPE_REPRESENTATION('',(#253),#6618);
#206=ADVANCED_BREP_SHAPE_REPRESENTATION('',(#254),#6619);
#207=ADVANCED_BREP_SHAPE_REPRESENTATION('',(#255),#6620);
#208=ADVANCED_BREP_SHAPE_REPRESENTATION('',(#256),#6621);
#209=ADVANCED_BREP_SHAPE_REPRESENTATION('',(#257),#6622);
#210=ADVANCED_BREP_SHAPE_REPRESENTATION('',(#258),#6623);
#211=ADVANCED_BREP_SHAPE_REPRESENTATION('',(#259),#6624);
#212=ADVANCED_BREP_SHAPE_REPRESENTATION('',(#260),#6625);
#213=ADVANCED_BREP_SHAPE_REPRESENTATION('',(#261),#6626);
#214=ADVANCED_BREP_SHAPE_REPRESENTATION('',(#171),#6627);
#215=ADVANCED_BREP_SHAPE_REPRESENTATION('',(#172),#6628);
#216=ADVANCED_BREP_SHAPE_REPRESENTATION('',(#262),#6630);
#217=ADVANCED_BREP_SHAPE_REPRESENTATION('',(#263),#6631);
#218=ADVANCED_BREP_SHAPE_REPRESENTATION('',(#264),#6632);
#219=ADVANCED_BREP_SHAPE_REPRESENTATION('',(#265),#6633);
#220=ADVANCED_BREP_SHAPE_REPRESENTATION('',(#266),#6634);
#221=ADVANCED_BREP_SHAPE_REPRESENTATION('',(#267),#6636);
#222=ADVANCED_BREP_SHAPE_REPRESENTATION('',(#268),#6637);
#223=STYLED_ITEM('',(#6922),#247);
#224=STYLED_ITEM('',(#6957),#248);
#225=STYLED_ITEM('',(#6957),#249);
#226=STYLED_ITEM('',(#6957),#250);
#227=STYLED_ITEM('',(#6957),#251);
#228=STYLED_ITEM('',(#6936),#252);
#229=STYLED_ITEM('',(#6929),#253);
#230=STYLED_ITEM('',(#6957),#254);
#231=STYLED_ITEM('',(#6957),#255);
#232=STYLED_ITEM('',(#6943),#256);
#233=STYLED_ITEM('',(#6943),#257);
#234=STYLED_ITEM('',(#6943),#258);
#235=STYLED_ITEM('',(#6957),#259);
#236=STYLED_ITEM('',(#6936),#260);
#237=STYLED_ITEM('',(#6936),#261);
#238=STYLED_ITEM('',(#6950),#171);
#239=STYLED_ITEM('',(#6950),#172);
#240=STYLED_ITEM('',(#6957),#262);
#241=STYLED_ITEM('',(#6957),#263);
#242=STYLED_ITEM('',(#6957),#264);
#243=STYLED_ITEM('',(#6929),#265);
#244=STYLED_ITEM('',(#6929),#266);
#245=STYLED_ITEM('',(#6936),#267);
#246=STYLED_ITEM('',(#6950),#268);
#247=MANIFOLD_SOLID_BREP('Body1',#3590);
#248=MANIFOLD_SOLID_BREP('Body1',#3591);
#249=MANIFOLD_SOLID_BREP('Body1',#3592);
#250=MANIFOLD_SOLID_BREP('Body1',#3593);
#251=MANIFOLD_SOLID_BREP('Body1',#3594);
#252=MANIFOLD_SOLID_BREP('Body1',#3595);
#253=MANIFOLD_SOLID_BREP('Body1',#3596);
#254=MANIFOLD_SOLID_BREP('Body1',#3597);
#255=MANIFOLD_SOLID_BREP('Body1',#3598);
#256=MANIFOLD_SOLID_BREP('Body1',#3599);
#257=MANIFOLD_SOLID_BREP('Body1',#3600);
#258=MANIFOLD_SOLID_BREP('Body1',#3601);
#259=MANIFOLD_SOLID_BREP('Body1',#3602);
#260=MANIFOLD_SOLID_BREP('Body1',#3603);
#261=MANIFOLD_SOLID_BREP('Body1',#3604);
#262=MANIFOLD_SOLID_BREP('Body1',#3609);
#263=MANIFOLD_SOLID_BREP('Body1',#3610);
#264=MANIFOLD_SOLID_BREP('Body1',#3611);
#265=MANIFOLD_SOLID_BREP('Body1',#3612);
#266=MANIFOLD_SOLID_BREP('Body1',#3613);
#267=MANIFOLD_SOLID_BREP('Body1',#3614);
#268=MANIFOLD_SOLID_BREP('Body1',#3615);
#269=FACE_BOUND('',#734,.T.);
#270=FACE_BOUND('',#735,.T.);
#271=FACE_BOUND('',#736,.T.);
#272=FACE_BOUND('',#737,.T.);
#273=FACE_BOUND('',#738,.T.);
#274=FACE_BOUND('',#739,.T.);
#275=FACE_BOUND('',#740,.T.);
#276=FACE_BOUND('',#741,.T.);
#277=FACE_BOUND('',#742,.T.);
#278=FACE_BOUND('',#743,.T.);
#279=FACE_BOUND('',#744,.T.);
#280=FACE_BOUND('',#745,.T.);
#281=FACE_BOUND('',#746,.T.);
#282=FACE_BOUND('',#747,.T.);
#283=FACE_BOUND('',#749,.T.);
#284=FACE_BOUND('',#750,.T.);
#285=FACE_BOUND('',#751,.T.);
#286=FACE_BOUND('',#752,.T.);
#287=FACE_BOUND('',#753,.T.);
#288=FACE_BOUND('',#754,.T.);
#289=FACE_BOUND('',#755,.T.);
#290=FACE_BOUND('',#756,.T.);
#291=FACE_BOUND('',#757,.T.);
#292=FACE_BOUND('',#758,.T.);
#293=FACE_BOUND('',#759,.T.);
#294=FACE_BOUND('',#760,.T.);
#295=FACE_BOUND('',#761,.T.);
#296=FACE_BOUND('',#762,.T.);
#297=FACE_BOUND('',#777,.T.);
#298=FACE_BOUND('',#780,.T.);
#299=FACE_BOUND('',#783,.T.);
#300=FACE_BOUND('',#786,.T.);
#301=FACE_BOUND('',#801,.T.);
#302=FACE_BOUND('',#802,.T.);
#303=FACE_BOUND('',#803,.T.);
#304=FACE_BOUND('',#804,.T.);
#305=FACE_BOUND('',#805,.T.);
#306=FACE_BOUND('',#807,.T.);
#307=FACE_BOUND('',#808,.T.);
#308=FACE_BOUND('',#809,.T.);
#309=FACE_BOUND('',#810,.T.);
#310=FACE_BOUND('',#818,.T.);
#311=FACE_BOUND('',#820,.T.);
#312=FACE_BOUND('',#824,.T.);
#313=FACE_BOUND('',#826,.T.);
#314=FACE_BOUND('',#829,.T.);
#315=FACE_BOUND('',#832,.T.);
#316=FACE_BOUND('',#833,.T.);
#317=FACE_BOUND('',#836,.T.);
#318=FACE_BOUND('',#838,.T.);
#319=FACE_BOUND('',#840,.T.);
#320=FACE_BOUND('',#842,.T.);
#321=FACE_BOUND('',#846,.T.);
#322=FACE_BOUND('',#848,.T.);
#323=FACE_BOUND('',#851,.T.);
#324=FACE_BOUND('',#854,.T.);
#325=FACE_BOUND('',#855,.T.);
#326=FACE_BOUND('',#858,.T.);
#327=FACE_BOUND('',#860,.T.);
#328=FACE_BOUND('',#867,.T.);
#329=FACE_BOUND('',#869,.T.);
#330=FACE_BOUND('',#873,.T.);
#331=FACE_BOUND('',#875,.T.);
#332=FACE_BOUND('',#879,.T.);
#333=FACE_BOUND('',#881,.T.);
#334=FACE_BOUND('',#890,.T.);
#335=FACE_BOUND('',#894,.T.);
#336=FACE_BOUND('',#896,.T.);
#337=FACE_BOUND('',#898,.T.);
#338=FACE_BOUND('',#899,.T.);
#339=FACE_BOUND('',#903,.T.);
#340=FACE_BOUND('',#905,.T.);
#341=FACE_BOUND('',#909,.T.);
#342=FACE_BOUND('',#911,.T.);
#343=FACE_BOUND('',#926,.T.);
#344=FACE_BOUND('',#943,.T.);
#345=FACE_BOUND('',#951,.T.);
#346=FACE_BOUND('',#954,.T.);
#347=FACE_BOUND('',#962,.T.);
#348=FACE_BOUND('',#963,.T.);
#349=FACE_BOUND('',#964,.T.);
#350=FACE_BOUND('',#965,.T.);
#351=FACE_BOUND('',#975,.T.);
#352=FACE_BOUND('',#976,.T.);
#353=FACE_BOUND('',#977,.T.);
#354=FACE_BOUND('',#978,.T.);
#355=FACE_BOUND('',#980,.T.);
#356=FACE_BOUND('',#983,.T.);
#357=FACE_BOUND('',#987,.T.);
#358=FACE_BOUND('',#989,.T.);
#359=FACE_BOUND('',#992,.T.);
#360=FACE_BOUND('',#996,.T.);
#361=FACE_BOUND('',#998,.T.);
#362=FACE_BOUND('',#1001,.T.);
#363=FACE_BOUND('',#1005,.T.);
#364=FACE_BOUND('',#1007,.T.);
#365=FACE_BOUND('',#1010,.T.);
#366=FACE_BOUND('',#1014,.T.);
#367=FACE_BOUND('',#1020,.T.);
#368=FACE_BOUND('',#1022,.T.);
#369=FACE_BOUND('',#1026,.T.);
#370=PLANE('',#3926);
#371=PLANE('',#3927);
#372=PLANE('',#3928);
#373=PLANE('',#3929);
#374=PLANE('',#3930);
#375=PLANE('',#3931);
#376=PLANE('',#3936);
#377=PLANE('',#3937);
#378=PLANE('',#3942);
#379=PLANE('',#3943);
#380=PLANE('',#3948);
#381=PLANE('',#3949);
#382=PLANE('',#3954);
#383=PLANE('',#3955);
#384=PLANE('',#3960);
#385=PLANE('',#3965);
#386=PLANE('',#3970);
#387=PLANE('',#3975);
#388=PLANE('',#3985);
#389=PLANE('',#3986);
#390=PLANE('',#3987);
#391=PLANE('',#3988);
#392=PLANE('',#3989);
#393=PLANE('',#3990);
#394=PLANE('',#3991);
#395=PLANE('',#3992);
#396=PLANE('',#3993);
#397=PLANE('',#3994);
#398=PLANE('',#3995);
#399=PLANE('',#3997);
#400=PLANE('',#3998);
#401=PLANE('',#3999);
#402=PLANE('',#4000);
#403=PLANE('',#4001);
#404=PLANE('',#4002);
#405=PLANE('',#4007);
#406=PLANE('',#4017);
#407=PLANE('',#4018);
#408=PLANE('',#4019);
#409=PLANE('',#4020);
#410=PLANE('',#4021);
#411=PLANE('',#4022);
#412=PLANE('',#4023);
#413=PLANE('',#4024);
#414=PLANE('',#4029);
#415=PLANE('',#4039);
#416=PLANE('',#4040);
#417=PLANE('',#4041);
#418=PLANE('',#4042);
#419=PLANE('',#4043);
#420=PLANE('',#4044);
#421=PLANE('',#4045);
#422=PLANE('',#4046);
#423=PLANE('',#4051);
#424=PLANE('',#4055);
#425=PLANE('',#4059);
#426=PLANE('',#4060);
#427=PLANE('',#4068);
#428=PLANE('',#4069);
#429=PLANE('',#4077);
#430=PLANE('',#4078);
#431=PLANE('',#4083);
#432=PLANE('',#4084);
#433=PLANE('',#4091);
#434=PLANE('',#4103);
#435=PLANE('',#4110);
#436=PLANE('',#4111);
#437=PLANE('',#4112);
#438=PLANE('',#4120);
#439=PLANE('',#4121);
#440=PLANE('',#4129);
#441=PLANE('',#4130);
#442=PLANE('',#4132);
#443=PLANE('',#4133);
#444=PLANE('',#4134);
#445=PLANE('',#4135);
#446=PLANE('',#4136);
#447=PLANE('',#4137);
#448=PLANE('',#4138);
#449=PLANE('',#4139);
#450=PLANE('',#4140);
#451=PLANE('',#4142);
#452=PLANE('',#4150);
#453=PLANE('',#4156);
#454=PLANE('',#4157);
#455=PLANE('',#4158);
#456=PLANE('',#4159);
#457=PLANE('',#4160);
#458=PLANE('',#4161);
#459=PLANE('',#4162);
#460=PLANE('',#4163);
#461=PLANE('',#4164);
#462=PLANE('',#4166);
#463=PLANE('',#4174);
#464=PLANE('',#4221);
#465=PLANE('',#4224);
#466=PLANE('',#4225);
#467=PLANE('',#4230);
#468=PLANE('',#4231);
#469=PLANE('',#4232);
#470=PLANE('',#4233);
#471=PLANE('',#4234);
#472=PLANE('',#4235);
#473=PLANE('',#4236);
#474=PLANE('',#4237);
#475=PLANE('',#4238);
#476=PLANE('',#4239);
#477=PLANE('',#4240);
#478=PLANE('',#4241);
#479=PLANE('',#4242);
#480=PLANE('',#4243);
#481=PLANE('',#4245);
#482=PLANE('',#4250);
#483=PLANE('',#4256);
#484=PLANE('',#4258);
#485=PLANE('',#4263);
#486=PLANE('',#4269);
#487=PLANE('',#4271);
#488=PLANE('',#4276);
#489=PLANE('',#4282);
#490=PLANE('',#4284);
#491=PLANE('',#4289);
#492=PLANE('',#4295);
#493=PLANE('',#4306);
#494=PLANE('',#4307);
#495=PLANE('',#4308);
#496=PLANE('',#4309);
#497=PLANE('',#4311);
#498=PLANE('',#4317);
#499=PLANE('',#4322);
#500=PLANE('',#4323);
#501=FACE_OUTER_BOUND('',#715,.T.);
#502=FACE_OUTER_BOUND('',#716,.T.);
#503=FACE_OUTER_BOUND('',#717,.T.);
#504=FACE_OUTER_BOUND('',#718,.T.);
#505=FACE_OUTER_BOUND('',#719,.T.);
#506=FACE_OUTER_BOUND('',#720,.T.);
#507=FACE_OUTER_BOUND('',#721,.T.);
#508=FACE_OUTER_BOUND('',#722,.T.);
#509=FACE_OUTER_BOUND('',#723,.T.);
#510=FACE_OUTER_BOUND('',#724,.T.);
#511=FACE_OUTER_BOUND('',#725,.T.);
#512=FACE_OUTER_BOUND('',#726,.T.);
#513=FACE_OUTER_BOUND('',#727,.T.);
#514=FACE_OUTER_BOUND('',#728,.T.);
#515=FACE_OUTER_BOUND('',#729,.T.);
#516=FACE_OUTER_BOUND('',#730,.T.);
#517=FACE_OUTER_BOUND('',#731,.T.);
#518=FACE_OUTER_BOUND('',#732,.T.);
#519=FACE_OUTER_BOUND('',#733,.T.);
#520=FACE_OUTER_BOUND('',#748,.T.);
#521=FACE_OUTER_BOUND('',#763,.T.);
#522=FACE_OUTER_BOUND('',#764,.T.);
#523=FACE_OUTER_BOUND('',#765,.T.);
#524=FACE_OUTER_BOUND('',#766,.T.);
#525=FACE_OUTER_BOUND('',#767,.T.);
#526=FACE_OUTER_BOUND('',#768,.T.);
#527=FACE_OUTER_BOUND('',#769,.T.);
#528=FACE_OUTER_BOUND('',#770,.T.);
#529=FACE_OUTER_BOUND('',#771,.T.);
#530=FACE_OUTER_BOUND('',#772,.T.);
#531=FACE_OUTER_BOUND('',#773,.T.);
#532=FACE_OUTER_BOUND('',#774,.T.);
#533=FACE_OUTER_BOUND('',#775,.T.);
#534=FACE_OUTER_BOUND('',#776,.T.);
#535=FACE_OUTER_BOUND('',#778,.T.);
#536=FACE_OUTER_BOUND('',#779,.T.);
#537=FACE_OUTER_BOUND('',#781,.T.);
#538=FACE_OUTER_BOUND('',#782,.T.);
#539=FACE_OUTER_BOUND('',#784,.T.);
#540=FACE_OUTER_BOUND('',#785,.T.);
#541=FACE_OUTER_BOUND('',#787,.T.);
#542=FACE_OUTER_BOUND('',#788,.T.);
#543=FACE_OUTER_BOUND('',#789,.T.);
#544=FACE_OUTER_BOUND('',#790,.T.);
#545=FACE_OUTER_BOUND('',#791,.T.);
#546=FACE_OUTER_BOUND('',#792,.T.);
#547=FACE_OUTER_BOUND('',#793,.T.);
#548=FACE_OUTER_BOUND('',#794,.T.);
#549=FACE_OUTER_BOUND('',#795,.T.);
#550=FACE_OUTER_BOUND('',#796,.T.);
#551=FACE_OUTER_BOUND('',#797,.T.);
#552=FACE_OUTER_BOUND('',#798,.T.);
#553=FACE_OUTER_BOUND('',#799,.T.);
#554=FACE_OUTER_BOUND('',#800,.T.);
#555=FACE_OUTER_BOUND('',#806,.T.);
#556=FACE_OUTER_BOUND('',#811,.T.);
#557=FACE_OUTER_BOUND('',#812,.T.);
#558=FACE_OUTER_BOUND('',#813,.T.);
#559=FACE_OUTER_BOUND('',#814,.T.);
#560=FACE_OUTER_BOUND('',#815,.T.);
#561=FACE_OUTER_BOUND('',#816,.T.);
#562=FACE_OUTER_BOUND('',#817,.T.);
#563=FACE_OUTER_BOUND('',#819,.T.);
#564=FACE_OUTER_BOUND('',#821,.T.);
#565=FACE_OUTER_BOUND('',#822,.T.);
#566=FACE_OUTER_BOUND('',#823,.T.);
#567=FACE_OUTER_BOUND('',#825,.T.);
#568=FACE_OUTER_BOUND('',#827,.T.);
#569=FACE_OUTER_BOUND('',#828,.T.);
#570=FACE_OUTER_BOUND('',#830,.T.);
#571=FACE_OUTER_BOUND('',#831,.T.);
#572=FACE_OUTER_BOUND('',#834,.T.);
#573=FACE_OUTER_BOUND('',#835,.T.);
#574=FACE_OUTER_BOUND('',#837,.T.);
#575=FACE_OUTER_BOUND('',#839,.T.);
#576=FACE_OUTER_BOUND('',#841,.T.);
#577=FACE_OUTER_BOUND('',#843,.T.);
#578=FACE_OUTER_BOUND('',#844,.T.);
#579=FACE_OUTER_BOUND('',#845,.T.);
#580=FACE_OUTER_BOUND('',#847,.T.);
#581=FACE_OUTER_BOUND('',#849,.T.);
#582=FACE_OUTER_BOUND('',#850,.T.);
#583=FACE_OUTER_BOUND('',#852,.T.);
#584=FACE_OUTER_BOUND('',#853,.T.);
#585=FACE_OUTER_BOUND('',#856,.T.);
#586=FACE_OUTER_BOUND('',#857,.T.);
#587=FACE_OUTER_BOUND('',#859,.T.);
#588=FACE_OUTER_BOUND('',#861,.T.);
#589=FACE_OUTER_BOUND('',#862,.T.);
#590=FACE_OUTER_BOUND('',#863,.T.);
#591=FACE_OUTER_BOUND('',#864,.T.);
#592=FACE_OUTER_BOUND('',#865,.T.);
#593=FACE_OUTER_BOUND('',#866,.T.);
#594=FACE_OUTER_BOUND('',#868,.T.);
#595=FACE_OUTER_BOUND('',#870,.T.);
#596=FACE_OUTER_BOUND('',#871,.T.);
#597=FACE_OUTER_BOUND('',#872,.T.);
#598=FACE_OUTER_BOUND('',#874,.T.);
#599=FACE_OUTER_BOUND('',#876,.T.);
#600=FACE_OUTER_BOUND('',#877,.T.);
#601=FACE_OUTER_BOUND('',#878,.T.);
#602=FACE_OUTER_BOUND('',#880,.T.);
#603=FACE_OUTER_BOUND('',#882,.T.);
#604=FACE_OUTER_BOUND('',#883,.T.);
#605=FACE_OUTER_BOUND('',#884,.T.);
#606=FACE_OUTER_BOUND('',#885,.T.);
#607=FACE_OUTER_BOUND('',#886,.T.);
#608=FACE_OUTER_BOUND('',#887,.T.);
#609=FACE_OUTER_BOUND('',#888,.T.);
#610=FACE_OUTER_BOUND('',#889,.T.);
#611=FACE_OUTER_BOUND('',#891,.T.);
#612=FACE_OUTER_BOUND('',#892,.T.);
#613=FACE_OUTER_BOUND('',#893,.T.);
#614=FACE_OUTER_BOUND('',#895,.T.);
#615=FACE_OUTER_BOUND('',#897,.T.);
#616=FACE_OUTER_BOUND('',#900,.T.);
#617=FACE_OUTER_BOUND('',#901,.T.);
#618=FACE_OUTER_BOUND('',#902,.T.);
#619=FACE_OUTER_BOUND('',#904,.T.);
#620=FACE_OUTER_BOUND('',#906,.T.);
#621=FACE_OUTER_BOUND('',#907,.T.);
#622=FACE_OUTER_BOUND('',#908,.T.);
#623=FACE_OUTER_BOUND('',#910,.T.);
#624=FACE_OUTER_BOUND('',#912,.T.);
#625=FACE_OUTER_BOUND('',#913,.T.);
#626=FACE_OUTER_BOUND('',#914,.T.);
#627=FACE_OUTER_BOUND('',#915,.T.);
#628=FACE_OUTER_BOUND('',#916,.T.);
#629=FACE_OUTER_BOUND('',#917,.T.);
#630=FACE_OUTER_BOUND('',#918,.T.);
#631=FACE_OUTER_BOUND('',#919,.T.);
#632=FACE_OUTER_BOUND('',#920,.T.);
#633=FACE_OUTER_BOUND('',#921,.T.);
#634=FACE_OUTER_BOUND('',#922,.T.);
#635=FACE_OUTER_BOUND('',#923,.T.);
#636=FACE_OUTER_BOUND('',#924,.T.);
#637=FACE_OUTER_BOUND('',#925,.T.);
#638=FACE_OUTER_BOUND('',#927,.T.);
#639=FACE_OUTER_BOUND('',#928,.T.);
#640=FACE_OUTER_BOUND('',#929,.T.);
#641=FACE_OUTER_BOUND('',#930,.T.);
#642=FACE_OUTER_BOUND('',#931,.T.);
#643=FACE_OUTER_BOUND('',#932,.T.);
#644=FACE_OUTER_BOUND('',#933,.T.);
#645=FACE_OUTER_BOUND('',#934,.T.);
#646=FACE_OUTER_BOUND('',#935,.T.);
#647=FACE_OUTER_BOUND('',#936,.T.);
#648=FACE_OUTER_BOUND('',#937,.T.);
#649=FACE_OUTER_BOUND('',#938,.T.);
#650=FACE_OUTER_BOUND('',#939,.T.);
#651=FACE_OUTER_BOUND('',#940,.T.);
#652=FACE_OUTER_BOUND('',#941,.T.);
#653=FACE_OUTER_BOUND('',#942,.T.);
#654=FACE_OUTER_BOUND('',#944,.T.);
#655=FACE_OUTER_BOUND('',#945,.T.);
#656=FACE_OUTER_BOUND('',#946,.T.);
#657=FACE_OUTER_BOUND('',#947,.T.);
#658=FACE_OUTER_BOUND('',#948,.T.);
#659=FACE_OUTER_BOUND('',#949,.T.);
#660=FACE_OUTER_BOUND('',#950,.T.);
#661=FACE_OUTER_BOUND('',#952,.T.);
#662=FACE_OUTER_BOUND('',#953,.T.);
#663=FACE_OUTER_BOUND('',#955,.T.);
#664=FACE_OUTER_BOUND('',#956,.T.);
#665=FACE_OUTER_BOUND('',#957,.T.);
#666=FACE_OUTER_BOUND('',#958,.T.);
#667=FACE_OUTER_BOUND('',#959,.T.);
#668=FACE_OUTER_BOUND('',#960,.T.);
#669=FACE_OUTER_BOUND('',#961,.T.);
#670=FACE_OUTER_BOUND('',#966,.T.);
#671=FACE_OUTER_BOUND('',#967,.T.);
#672=FACE_OUTER_BOUND('',#968,.T.);
#673=FACE_OUTER_BOUND('',#969,.T.);
#674=FACE_OUTER_BOUND('',#970,.T.);
#675=FACE_OUTER_BOUND('',#971,.T.);
#676=FACE_OUTER_BOUND('',#972,.T.);
#677=FACE_OUTER_BOUND('',#973,.T.);
#678=FACE_OUTER_BOUND('',#974,.T.);
#679=FACE_OUTER_BOUND('',#979,.T.);
#680=FACE_OUTER_BOUND('',#981,.T.);
#681=FACE_OUTER_BOUND('',#982,.T.);
#682=FACE_OUTER_BOUND('',#984,.T.);
#683=FACE_OUTER_BOUND('',#985,.T.);
#684=FACE_OUTER_BOUND('',#986,.T.);
#685=FACE_OUTER_BOUND('',#988,.T.);
#686=FACE_OUTER_BOUND('',#990,.T.);
#687=FACE_OUTER_BOUND('',#991,.T.);
#688=FACE_OUTER_BOUND('',#993,.T.);
#689=FACE_OUTER_BOUND('',#994,.T.);
#690=FACE_OUTER_BOUND('',#995,.T.);
#691=FACE_OUTER_BOUND('',#997,.T.);
#692=FACE_OUTER_BOUND('',#999,.T.);
#693=FACE_OUTER_BOUND('',#1000,.T.);
#694=FACE_OUTER_BOUND('',#1002,.T.);
#695=FACE_OUTER_BOUND('',#1003,.T.);
#696=FACE_OUTER_BOUND('',#1004,.T.);
#697=FACE_OUTER_BOUND('',#1006,.T.);
#698=FACE_OUTER_BOUND('',#1008,.T.);
#699=FACE_OUTER_BOUND('',#1009,.T.);
#700=FACE_OUTER_BOUND('',#1011,.T.);
#701=FACE_OUTER_BOUND('',#1012,.T.);
#702=FACE_OUTER_BOUND('',#1013,.T.);
#703=FACE_OUTER_BOUND('',#1015,.T.);
#704=FACE_OUTER_BOUND('',#1016,.T.);
#705=FACE_OUTER_BOUND('',#1017,.T.);
#706=FACE_OUTER_BOUND('',#1018,.T.);
#707=FACE_OUTER_BOUND('',#1019,.T.);
#708=FACE_OUTER_BOUND('',#1021,.T.);
#709=FACE_OUTER_BOUND('',#1023,.T.);
#710=FACE_OUTER_BOUND('',#1024,.T.);
#711=FACE_OUTER_BOUND('',#1025,.T.);
#712=FACE_OUTER_BOUND('',#1027,.T.);
#713=FACE_OUTER_BOUND('',#1028,.T.);
#714=FACE_OUTER_BOUND('',#1029,.T.);
#715=EDGE_LOOP('',(#2437,#2438,#2439,#2440));
#716=EDGE_LOOP('',(#2441,#2442,#2443,#2444));
#717=EDGE_LOOP('',(#2445,#2446,#2447,#2448));
#718=EDGE_LOOP('',(#2449,#2450,#2451,#2452));
#719=EDGE_LOOP('',(#2453,#2454,#2455,#2456));
#720=EDGE_LOOP('',(#2457,#2458,#2459,#2460));
#721=EDGE_LOOP('',(#2461,#2462,#2463,#2464));
#722=EDGE_LOOP('',(#2465,#2466,#2467,#2468));
#723=EDGE_LOOP('',(#2469,#2470,#2471,#2472));
#724=EDGE_LOOP('',(#2473,#2474,#2475,#2476));
#725=EDGE_LOOP('',(#2477,#2478,#2479,#2480));
#726=EDGE_LOOP('',(#2481,#2482,#2483,#2484));
#727=EDGE_LOOP('',(#2485,#2486,#2487,#2488));
#728=EDGE_LOOP('',(#2489,#2490,#2491,#2492));
#729=EDGE_LOOP('',(#2493,#2494,#2495,#2496));
#730=EDGE_LOOP('',(#2497,#2498,#2499,#2500));
#731=EDGE_LOOP('',(#2501,#2502,#2503,#2504));
#732=EDGE_LOOP('',(#2505,#2506,#2507,#2508));
#733=EDGE_LOOP('',(#2509,#2510,#2511,#2512));
#734=EDGE_LOOP('',(#2513));
#735=EDGE_LOOP('',(#2514));
#736=EDGE_LOOP('',(#2515));
#737=EDGE_LOOP('',(#2516));
#738=EDGE_LOOP('',(#2517));
#739=EDGE_LOOP('',(#2518));
#740=EDGE_LOOP('',(#2519));
#741=EDGE_LOOP('',(#2520));
#742=EDGE_LOOP('',(#2521));
#743=EDGE_LOOP('',(#2522));
#744=EDGE_LOOP('',(#2523));
#745=EDGE_LOOP('',(#2524));
#746=EDGE_LOOP('',(#2525));
#747=EDGE_LOOP('',(#2526));
#748=EDGE_LOOP('',(#2527,#2528,#2529,#2530));
#749=EDGE_LOOP('',(#2531));
#750=EDGE_LOOP('',(#2532));
#751=EDGE_LOOP('',(#2533));
#752=EDGE_LOOP('',(#2534));
#753=EDGE_LOOP('',(#2535));
#754=EDGE_LOOP('',(#2536));
#755=EDGE_LOOP('',(#2537));
#756=EDGE_LOOP('',(#2538));
#757=EDGE_LOOP('',(#2539));
#758=EDGE_LOOP('',(#2540));
#759=EDGE_LOOP('',(#2541));
#760=EDGE_LOOP('',(#2542));
#761=EDGE_LOOP('',(#2543));
#762=EDGE_LOOP('',(#2544));
#763=EDGE_LOOP('',(#2545,#2546,#2547,#2548));
#764=EDGE_LOOP('',(#2549));
#765=EDGE_LOOP('',(#2550));
#766=EDGE_LOOP('',(#2551,#2552,#2553,#2554));
#767=EDGE_LOOP('',(#2555));
#768=EDGE_LOOP('',(#2556));
#769=EDGE_LOOP('',(#2557,#2558,#2559,#2560));
#770=EDGE_LOOP('',(#2561));
#771=EDGE_LOOP('',(#2562));
#772=EDGE_LOOP('',(#2563,#2564,#2565,#2566));
#773=EDGE_LOOP('',(#2567));
#774=EDGE_LOOP('',(#2568));
#775=EDGE_LOOP('',(#2569,#2570,#2571,#2572));
#776=EDGE_LOOP('',(#2573));
#777=EDGE_LOOP('',(#2574));
#778=EDGE_LOOP('',(#2575,#2576,#2577,#2578));
#779=EDGE_LOOP('',(#2579));
#780=EDGE_LOOP('',(#2580));
#781=EDGE_LOOP('',(#2581,#2582,#2583,#2584));
#782=EDGE_LOOP('',(#2585));
#783=EDGE_LOOP('',(#2586));
#784=EDGE_LOOP('',(#2587,#2588,#2589,#2590));
#785=EDGE_LOOP('',(#2591));
#786=EDGE_LOOP('',(#2592));
#787=EDGE_LOOP('',(#2593,#2594,#2595,#2596));
#788=EDGE_LOOP('',(#2597,#2598,#2599,#2600));
#789=EDGE_LOOP('',(#2601,#2602,#2603,#2604));
#790=EDGE_LOOP('',(#2605,#2606,#2607,#2608));
#791=EDGE_LOOP('',(#2609,#2610,#2611,#2612));
#792=EDGE_LOOP('',(#2613,#2614,#2615,#2616));
#793=EDGE_LOOP('',(#2617,#2618,#2619,#2620));
#794=EDGE_LOOP('',(#2621,#2622,#2623,#2624));
#795=EDGE_LOOP('',(#2625,#2626,#2627,#2628));
#796=EDGE_LOOP('',(#2629,#2630,#2631,#2632));
#797=EDGE_LOOP('',(#2633,#2634,#2635,#2636));
#798=EDGE_LOOP('',(#2637,#2638,#2639,#2640));
#799=EDGE_LOOP('',(#2641,#2642,#2643,#2644));
#800=EDGE_LOOP('',(#2645,#2646,#2647,#2648));
#801=EDGE_LOOP('',(#2649,#2650,#2651,#2652));
#802=EDGE_LOOP('',(#2653));
#803=EDGE_LOOP('',(#2654));
#804=EDGE_LOOP('',(#2655));
#805=EDGE_LOOP('',(#2656));
#806=EDGE_LOOP('',(#2657,#2658,#2659,#2660));
#807=EDGE_LOOP('',(#2661));
#808=EDGE_LOOP('',(#2662));
#809=EDGE_LOOP('',(#2663));
#810=EDGE_LOOP('',(#2664));
#811=EDGE_LOOP('',(#2665,#2666,#2667,#2668));
#812=EDGE_LOOP('',(#2669,#2670,#2671,#2672));
#813=EDGE_LOOP('',(#2673,#2674,#2675,#2676));
#814=EDGE_LOOP('',(#2677,#2678,#2679,#2680));
#815=EDGE_LOOP('',(#2681,#2682,#2683,#2684));
#816=EDGE_LOOP('',(#2685,#2686,#2687,#2688));
#817=EDGE_LOOP('',(#2689,#2690,#2691,#2692));
#818=EDGE_LOOP('',(#2693));
#819=EDGE_LOOP('',(#2694));
#820=EDGE_LOOP('',(#2695));
#821=EDGE_LOOP('',(#2696,#2697,#2698,#2699));
#822=EDGE_LOOP('',(#2700,#2701,#2702,#2703));
#823=EDGE_LOOP('',(#2704,#2705,#2706,#2707));
#824=EDGE_LOOP('',(#2708));
#825=EDGE_LOOP('',(#2709,#2710,#2711,#2712));
#826=EDGE_LOOP('',(#2713));
#827=EDGE_LOOP('',(#2714,#2715,#2716,#2717));
#828=EDGE_LOOP('',(#2718,#2719,#2720,#2721));
#829=EDGE_LOOP('',(#2722));
#830=EDGE_LOOP('',(#2723,#2724,#2725,#2726));
#831=EDGE_LOOP('',(#2727,#2728,#2729,#2730));
#832=EDGE_LOOP('',(#2731));
#833=EDGE_LOOP('',(#2732));
#834=EDGE_LOOP('',(#2733,#2734,#2735,#2736));
#835=EDGE_LOOP('',(#2737,#2738,#2739,#2740,#2741,#2742));
#836=EDGE_LOOP('',(#2743));
#837=EDGE_LOOP('',(#2744,#2745,#2746,#2747,#2748,#2749));
#838=EDGE_LOOP('',(#2750));
#839=EDGE_LOOP('',(#2751,#2752,#2753,#2754));
#840=EDGE_LOOP('',(#2755));
#841=EDGE_LOOP('',(#2756));
#842=EDGE_LOOP('',(#2757));
#843=EDGE_LOOP('',(#2758,#2759,#2760,#2761));
#844=EDGE_LOOP('',(#2762,#2763,#2764,#2765));
#845=EDGE_LOOP('',(#2766,#2767,#2768,#2769));
#846=EDGE_LOOP('',(#2770));
#847=EDGE_LOOP('',(#2771,#2772,#2773,#2774));
#848=EDGE_LOOP('',(#2775));
#849=EDGE_LOOP('',(#2776,#2777,#2778,#2779));
#850=EDGE_LOOP('',(#2780,#2781,#2782,#2783));
#851=EDGE_LOOP('',(#2784));
#852=EDGE_LOOP('',(#2785,#2786,#2787,#2788));
#853=EDGE_LOOP('',(#2789,#2790,#2791,#2792));
#854=EDGE_LOOP('',(#2793));
#855=EDGE_LOOP('',(#2794));
#856=EDGE_LOOP('',(#2795,#2796,#2797,#2798));
#857=EDGE_LOOP('',(#2799,#2800,#2801,#2802,#2803,#2804));
#858=EDGE_LOOP('',(#2805));
#859=EDGE_LOOP('',(#2806,#2807,#2808,#2809,#2810,#2811));
#860=EDGE_LOOP('',(#2812));
#861=EDGE_LOOP('',(#2813,#2814,#2815,#2816));
#862=EDGE_LOOP('',(#2817));
#863=EDGE_LOOP('',(#2818,#2819,#2820,#2821));
#864=EDGE_LOOP('',(#2822));
#865=EDGE_LOOP('',(#2823,#2824,#2825,#2826));
#866=EDGE_LOOP('',(#2827));
#867=EDGE_LOOP('',(#2828));
#868=EDGE_LOOP('',(#2829));
#869=EDGE_LOOP('',(#2830));
#870=EDGE_LOOP('',(#2831,#2832,#2833,#2834));
#871=EDGE_LOOP('',(#2835,#2836,#2837,#2838));
#872=EDGE_LOOP('',(#2839));
#873=EDGE_LOOP('',(#2840));
#874=EDGE_LOOP('',(#2841));
#875=EDGE_LOOP('',(#2842));
#876=EDGE_LOOP('',(#2843,#2844,#2845,#2846));
#877=EDGE_LOOP('',(#2847,#2848,#2849,#2850));
#878=EDGE_LOOP('',(#2851));
#879=EDGE_LOOP('',(#2852));
#880=EDGE_LOOP('',(#2853));
#881=EDGE_LOOP('',(#2854));
#882=EDGE_LOOP('',(#2855,#2856,#2857,#2858));
#883=EDGE_LOOP('',(#2859));
#884=EDGE_LOOP('',(#2860,#2861));
#885=EDGE_LOOP('',(#2862,#2863,#2864,#2865,#2866,#2867,#2868,#2869));
#886=EDGE_LOOP('',(#2870,#2871));
#887=EDGE_LOOP('',(#2872,#2873,#2874,#2875,#2876,#2877,#2878,#2879));
#888=EDGE_LOOP('',(#2880,#2881,#2882,#2883,#2884,#2885,#2886,#2887,#2888,
#2889,#2890,#2891));
#889=EDGE_LOOP('',(#2892));
#890=EDGE_LOOP('',(#2893,#2894,#2895,#2896,#2897,#2898,#2899));
#891=EDGE_LOOP('',(#2900,#2901,#2902,#2903));
#892=EDGE_LOOP('',(#2904,#2905,#2906,#2907));
#893=EDGE_LOOP('',(#2908));
#894=EDGE_LOOP('',(#2909));
#895=EDGE_LOOP('',(#2910));
#896=EDGE_LOOP('',(#2911));
#897=EDGE_LOOP('',(#2912));
#898=EDGE_LOOP('',(#2913));
#899=EDGE_LOOP('',(#2914));
#900=EDGE_LOOP('',(#2915,#2916,#2917,#2918));
#901=EDGE_LOOP('',(#2919,#2920,#2921,#2922));
#902=EDGE_LOOP('',(#2923));
#903=EDGE_LOOP('',(#2924));
#904=EDGE_LOOP('',(#2925));
#905=EDGE_LOOP('',(#2926));
#906=EDGE_LOOP('',(#2927,#2928,#2929,#2930));
#907=EDGE_LOOP('',(#2931,#2932,#2933,#2934));
#908=EDGE_LOOP('',(#2935));
#909=EDGE_LOOP('',(#2936));
#910=EDGE_LOOP('',(#2937));
#911=EDGE_LOOP('',(#2938));
#912=EDGE_LOOP('',(#2939,#2940,#2941,#2942));
#913=EDGE_LOOP('',(#2943,#2944,#2945,#2946));
#914=EDGE_LOOP('',(#2947,#2948,#2949,#2950));
#915=EDGE_LOOP('',(#2951,#2952,#2953,#2954));
#916=EDGE_LOOP('',(#2955,#2956,#2957,#2958));
#917=EDGE_LOOP('',(#2959,#2960,#2961,#2962));
#918=EDGE_LOOP('',(#2963,#2964,#2965,#2966,#2967,#2968));
#919=EDGE_LOOP('',(#2969,#2970,#2971,#2972,#2973,#2974));
#920=EDGE_LOOP('',(#2975));
#921=EDGE_LOOP('',(#2976));
#922=EDGE_LOOP('',(#2977,#2978,#2979,#2980));
#923=EDGE_LOOP('',(#2981,#2982,#2983,#2984));
#924=EDGE_LOOP('',(#2985,#2986,#2987,#2988));
#925=EDGE_LOOP('',(#2989));
#926=EDGE_LOOP('',(#2990));
#927=EDGE_LOOP('',(#2991,#2992,#2993,#2994));
#928=EDGE_LOOP('',(#2995,#2996,#2997,#2998));
#929=EDGE_LOOP('',(#2999,#3000,#3001,#3002));
#930=EDGE_LOOP('',(#3003,#3004,#3005,#3006));
#931=EDGE_LOOP('',(#3007,#3008,#3009,#3010));
#932=EDGE_LOOP('',(#3011,#3012,#3013,#3014));
#933=EDGE_LOOP('',(#3015,#3016,#3017,#3018));
#934=EDGE_LOOP('',(#3019,#3020,#3021,#3022));
#935=EDGE_LOOP('',(#3023,#3024,#3025,#3026,#3027,#3028));
#936=EDGE_LOOP('',(#3029,#3030,#3031,#3032,#3033,#3034));
#937=EDGE_LOOP('',(#3035));
#938=EDGE_LOOP('',(#3036));
#939=EDGE_LOOP('',(#3037,#3038,#3039,#3040));
#940=EDGE_LOOP('',(#3041,#3042,#3043,#3044));
#941=EDGE_LOOP('',(#3045,#3046,#3047,#3048));
#942=EDGE_LOOP('',(#3049));
#943=EDGE_LOOP('',(#3050));
#944=EDGE_LOOP('',(#3051,#3052,#3053,#3054));
#945=EDGE_LOOP('',(#3055,#3056,#3057,#3058));
#946=EDGE_LOOP('',(#3059,#3060,#3061,#3062));
#947=EDGE_LOOP('',(#3063,#3064,#3065,#3066));
#948=EDGE_LOOP('',(#3067,#3068,#3069,#3070));
#949=EDGE_LOOP('',(#3071,#3072,#3073,#3074));
#950=EDGE_LOOP('',(#3075,#3076,#3077,#3078));
#951=EDGE_LOOP('',(#3079));
#952=EDGE_LOOP('',(#3080,#3081,#3082,#3083));
#953=EDGE_LOOP('',(#3084,#3085,#3086,#3087));
#954=EDGE_LOOP('',(#3088));
#955=EDGE_LOOP('',(#3089,#3090,#3091,#3092));
#956=EDGE_LOOP('',(#3093,#3094,#3095,#3096));
#957=EDGE_LOOP('',(#3097,#3098,#3099,#3100,#3101,#3102,#3103,#3104));
#958=EDGE_LOOP('',(#3105,#3106,#3107,#3108));
#959=EDGE_LOOP('',(#3109,#3110,#3111,#3112));
#960=EDGE_LOOP('',(#3113,#3114,#3115,#3116));
#961=EDGE_LOOP('',(#3117,#3118,#3119,#3120,#3121,#3122,#3123,#3124,#3125,
#3126,#3127,#3128,#3129,#3130,#3131,#3132));
#962=EDGE_LOOP('',(#3133));
#963=EDGE_LOOP('',(#3134));
#964=EDGE_LOOP('',(#3135));
#965=EDGE_LOOP('',(#3136));
#966=EDGE_LOOP('',(#3137,#3138,#3139,#3140));
#967=EDGE_LOOP('',(#3141,#3142,#3143,#3144));
#968=EDGE_LOOP('',(#3145,#3146,#3147,#3148));
#969=EDGE_LOOP('',(#3149,#3150,#3151,#3152));
#970=EDGE_LOOP('',(#3153,#3154,#3155,#3156));
#971=EDGE_LOOP('',(#3157,#3158,#3159,#3160));
#972=EDGE_LOOP('',(#3161,#3162,#3163,#3164));
#973=EDGE_LOOP('',(#3165,#3166,#3167,#3168));
#974=EDGE_LOOP('',(#3169,#3170,#3171,#3172,#3173,#3174,#3175,#3176,#3177,
#3178,#3179,#3180));
#975=EDGE_LOOP('',(#3181));
#976=EDGE_LOOP('',(#3182));
#977=EDGE_LOOP('',(#3183));
#978=EDGE_LOOP('',(#3184));
#979=EDGE_LOOP('',(#3185));
#980=EDGE_LOOP('',(#3186));
#981=EDGE_LOOP('',(#3187,#3188,#3189,#3190));
#982=EDGE_LOOP('',(#3191));
#983=EDGE_LOOP('',(#3192));
#984=EDGE_LOOP('',(#3193,#3194,#3195,#3196));
#985=EDGE_LOOP('',(#3197,#3198,#3199,#3200));
#986=EDGE_LOOP('',(#3201));
#987=EDGE_LOOP('',(#3202));
#988=EDGE_LOOP('',(#3203));
#989=EDGE_LOOP('',(#3204));
#990=EDGE_LOOP('',(#3205,#3206,#3207,#3208));
#991=EDGE_LOOP('',(#3209));
#992=EDGE_LOOP('',(#3210));
#993=EDGE_LOOP('',(#3211,#3212,#3213,#3214));
#994=EDGE_LOOP('',(#3215,#3216,#3217,#3218));
#995=EDGE_LOOP('',(#3219));
#996=EDGE_LOOP('',(#3220));
#997=EDGE_LOOP('',(#3221));
#998=EDGE_LOOP('',(#3222));
#999=EDGE_LOOP('',(#3223,#3224,#3225,#3226));
#1000=EDGE_LOOP('',(#3227));
#1001=EDGE_LOOP('',(#3228));
#1002=EDGE_LOOP('',(#3229,#3230,#3231,#3232));
#1003=EDGE_LOOP('',(#3233,#3234,#3235,#3236));
#1004=EDGE_LOOP('',(#3237));
#1005=EDGE_LOOP('',(#3238));
#1006=EDGE_LOOP('',(#3239));
#1007=EDGE_LOOP('',(#3240));
#1008=EDGE_LOOP('',(#3241,#3242,#3243,#3244));
#1009=EDGE_LOOP('',(#3245));
#1010=EDGE_LOOP('',(#3246));
#1011=EDGE_LOOP('',(#3247,#3248,#3249,#3250));
#1012=EDGE_LOOP('',(#3251,#3252,#3253,#3254));
#1013=EDGE_LOOP('',(#3255));
#1014=EDGE_LOOP('',(#3256));
#1015=EDGE_LOOP('',(#3257,#3258,#3259,#3260));
#1016=EDGE_LOOP('',(#3261,#3262,#3263,#3264));
#1017=EDGE_LOOP('',(#3265,#3266,#3267,#3268));
#1018=EDGE_LOOP('',(#3269,#3270,#3271,#3272));
#1019=EDGE_LOOP('',(#3273,#3274,#3275,#3276));
#1020=EDGE_LOOP('',(#3277));
#1021=EDGE_LOOP('',(#3278,#3279,#3280,#3281));
#1022=EDGE_LOOP('',(#3282));
#1023=EDGE_LOOP('',(#3283,#3284,#3285,#3286));
#1024=EDGE_LOOP('',(#3287,#3288,#3289,#3290));
#1025=EDGE_LOOP('',(#3291));
#1026=EDGE_LOOP('',(#3292));
#1027=EDGE_LOOP('',(#3293,#3294,#3295,#3296));
#1028=EDGE_LOOP('',(#3297));
#1029=EDGE_LOOP('',(#3298));
#1030=LINE('',#5493,#1291);
#1031=LINE('',#5499,#1292);
#1032=LINE('',#5505,#1293);
#1033=LINE('',#5511,#1294);
#1034=LINE('',#5517,#1295);
#1035=LINE('',#5523,#1296);
#1036=LINE('',#5529,#1297);
#1037=LINE('',#5535,#1298);
#1038=LINE('',#5541,#1299);
#1039=LINE('',#5547,#1300);
#1040=LINE('',#5553,#1301);
#1041=LINE('',#5559,#1302);
#1042=LINE('',#5565,#1303);
#1043=LINE('',#5571,#1304);
#1044=LINE('',#5576,#1305);
#1045=LINE('',#5578,#1306);
#1046=LINE('',#5580,#1307);
#1047=LINE('',#5581,#1308);
#1048=LINE('',#5584,#1309);
#1049=LINE('',#5586,#1310);
#1050=LINE('',#5587,#1311);
#1051=LINE('',#5590,#1312);
#1052=LINE('',#5592,#1313);
#1053=LINE('',#5593,#1314);
#1054=LINE('',#5595,#1315);
#1055=LINE('',#5596,#1316);
#1056=LINE('',#5604,#1317);
#1057=LINE('',#5613,#1318);
#1058=LINE('',#5622,#1319);
#1059=LINE('',#5631,#1320);
#1060=LINE('',#5640,#1321);
#1061=LINE('',#5649,#1322);
#1062=LINE('',#5658,#1323);
#1063=LINE('',#5667,#1324);
#1064=LINE('',#5675,#1325);
#1065=LINE('',#5679,#1326);
#1066=LINE('',#5683,#1327);
#1067=LINE('',#5687,#1328);
#1068=LINE('',#5691,#1329);
#1069=LINE('',#5693,#1330);
#1070=LINE('',#5695,#1331);
#1071=LINE('',#5696,#1332);
#1072=LINE('',#5699,#1333);
#1073=LINE('',#5701,#1334);
#1074=LINE('',#5702,#1335);
#1075=LINE('',#5705,#1336);
#1076=LINE('',#5707,#1337);
#1077=LINE('',#5708,#1338);
#1078=LINE('',#5710,#1339);
#1079=LINE('',#5711,#1340);
#1080=LINE('',#5716,#1341);
#1081=LINE('',#5718,#1342);
#1082=LINE('',#5720,#1343);
#1083=LINE('',#5721,#1344);
#1084=LINE('',#5724,#1345);
#1085=LINE('',#5726,#1346);
#1086=LINE('',#5727,#1347);
#1087=LINE('',#5730,#1348);
#1088=LINE('',#5732,#1349);
#1089=LINE('',#5733,#1350);
#1090=LINE('',#5735,#1351);
#1091=LINE('',#5736,#1352);
#1092=LINE('',#5743,#1353);
#1093=LINE('',#5745,#1354);
#1094=LINE('',#5747,#1355);
#1095=LINE('',#5748,#1356);
#1096=LINE('',#5751,#1357);
#1097=LINE('',#5753,#1358);
#1098=LINE('',#5754,#1359);
#1099=LINE('',#5757,#1360);
#1100=LINE('',#5759,#1361);
#1101=LINE('',#5760,#1362);
#1102=LINE('',#5762,#1363);
#1103=LINE('',#5763,#1364);
#1104=LINE('',#5771,#1365);
#1105=LINE('',#5830,#1366);
#1106=LINE('',#5835,#1367);
#1107=LINE('',#5841,#1368);
#1108=LINE('',#5846,#1369);
#1109=LINE('',#5848,#1370);
#1110=LINE('',#5850,#1371);
#1111=LINE('',#5851,#1372);
#1112=LINE('',#5854,#1373);
#1113=LINE('',#5856,#1374);
#1114=LINE('',#5857,#1375);
#1115=LINE('',#5860,#1376);
#1116=LINE('',#5862,#1377);
#1117=LINE('',#5863,#1378);
#1118=LINE('',#5866,#1379);
#1119=LINE('',#5868,#1380);
#1120=LINE('',#5869,#1381);
#1121=LINE('',#5872,#1382);
#1122=LINE('',#5874,#1383);
#1123=LINE('',#5875,#1384);
#1124=LINE('',#5877,#1385);
#1125=LINE('',#5878,#1386);
#1126=LINE('',#5886,#1387);
#1127=LINE('',#5945,#1388);
#1128=LINE('',#5950,#1389);
#1129=LINE('',#5956,#1390);
#1130=LINE('',#5961,#1391);
#1131=LINE('',#5963,#1392);
#1132=LINE('',#5965,#1393);
#1133=LINE('',#5966,#1394);
#1134=LINE('',#5969,#1395);
#1135=LINE('',#5971,#1396);
#1136=LINE('',#5972,#1397);
#1137=LINE('',#5975,#1398);
#1138=LINE('',#5977,#1399);
#1139=LINE('',#5978,#1400);
#1140=LINE('',#5981,#1401);
#1141=LINE('',#5983,#1402);
#1142=LINE('',#5984,#1403);
#1143=LINE('',#5987,#1404);
#1144=LINE('',#5989,#1405);
#1145=LINE('',#5990,#1406);
#1146=LINE('',#5992,#1407);
#1147=LINE('',#5993,#1408);
#1148=LINE('',#6001,#1409);
#1149=LINE('',#6008,#1410);
#1150=LINE('',#6015,#1411);
#1151=LINE('',#6024,#1412);
#1152=LINE('',#6030,#1413);
#1153=LINE('',#6039,#1414);
#1154=LINE('',#6045,#1415);
#1155=LINE('',#6054,#1416);
#1156=LINE('',#6066,#1417);
#1157=LINE('',#6069,#1418);
#1158=LINE('',#6071,#1419);
#1159=LINE('',#6082,#1420);
#1160=LINE('',#6085,#1421);
#1161=LINE('',#6087,#1422);
#1162=LINE('',#6093,#1423);
#1163=LINE('',#6102,#1424);
#1164=LINE('',#6108,#1425);
#1165=LINE('',#6118,#1426);
#1166=LINE('',#6124,#1427);
#1167=LINE('',#6133,#1428);
#1168=LINE('',#6139,#1429);
#1169=LINE('',#6147,#1430);
#1170=LINE('',#6149,#1431);
#1171=LINE('',#6151,#1432);
#1172=LINE('',#6152,#1433);
#1173=LINE('',#6155,#1434);
#1174=LINE('',#6157,#1435);
#1175=LINE('',#6158,#1436);
#1176=LINE('',#6161,#1437);
#1177=LINE('',#6163,#1438);
#1178=LINE('',#6164,#1439);
#1179=LINE('',#6167,#1440);
#1180=LINE('',#6169,#1441);
#1181=LINE('',#6170,#1442);
#1182=LINE('',#6173,#1443);
#1183=LINE('',#6175,#1444);
#1184=LINE('',#6176,#1445);
#1185=LINE('',#6178,#1446);
#1186=LINE('',#6179,#1447);
#1187=LINE('',#6191,#1448);
#1188=LINE('',#6195,#1449);
#1189=LINE('',#6199,#1450);
#1190=LINE('',#6206,#1451);
#1191=LINE('',#6208,#1452);
#1192=LINE('',#6213,#1453);
#1193=LINE('',#6215,#1454);
#1194=LINE('',#6217,#1455);
#1195=LINE('',#6218,#1456);
#1196=LINE('',#6221,#1457);
#1197=LINE('',#6223,#1458);
#1198=LINE('',#6224,#1459);
#1199=LINE('',#6227,#1460);
#1200=LINE('',#6229,#1461);
#1201=LINE('',#6230,#1462);
#1202=LINE('',#6233,#1463);
#1203=LINE('',#6235,#1464);
#1204=LINE('',#6236,#1465);
#1205=LINE('',#6239,#1466);
#1206=LINE('',#6241,#1467);
#1207=LINE('',#6242,#1468);
#1208=LINE('',#6244,#1469);
#1209=LINE('',#6245,#1470);
#1210=LINE('',#6257,#1471);
#1211=LINE('',#6261,#1472);
#1212=LINE('',#6265,#1473);
#1213=LINE('',#6272,#1474);
#1214=LINE('',#6274,#1475);
#1215=LINE('',#6309,#1476);
#1216=LINE('',#6315,#1477);
#1217=LINE('',#6321,#1478);
#1218=LINE('',#6327,#1479);
#1219=LINE('',#6334,#1480);
#1220=LINE('',#6336,#1481);
#1221=LINE('',#6337,#1482);
#1222=LINE('',#6342,#1483);
#1223=LINE('',#6344,#1484);
#1224=LINE('',#6345,#1485);
#1225=LINE('',#6350,#1486);
#1226=LINE('',#6351,#1487);
#1227=LINE('',#6355,#1488);
#1228=LINE('',#6357,#1489);
#1229=LINE('',#6360,#1490);
#1230=LINE('',#6362,#1491);
#1231=LINE('',#6364,#1492);
#1232=LINE('',#6366,#1493);
#1233=LINE('',#6367,#1494);
#1234=LINE('',#6370,#1495);
#1235=LINE('',#6372,#1496);
#1236=LINE('',#6373,#1497);
#1237=LINE('',#6376,#1498);
#1238=LINE('',#6378,#1499);
#1239=LINE('',#6379,#1500);
#1240=LINE('',#6382,#1501);
#1241=LINE('',#6384,#1502);
#1242=LINE('',#6385,#1503);
#1243=LINE('',#6388,#1504);
#1244=LINE('',#6390,#1505);
#1245=LINE('',#6392,#1506);
#1246=LINE('',#6394,#1507);
#1247=LINE('',#6396,#1508);
#1248=LINE('',#6398,#1509);
#1249=LINE('',#6400,#1510);
#1250=LINE('',#6401,#1511);
#1251=LINE('',#6404,#1512);
#1252=LINE('',#6405,#1513);
#1253=LINE('',#6408,#1514);
#1254=LINE('',#6409,#1515);
#1255=LINE('',#6412,#1516);
#1256=LINE('',#6413,#1517);
#1257=LINE('',#6416,#1518);
#1258=LINE('',#6417,#1519);
#1259=LINE('',#6420,#1520);
#1260=LINE('',#6421,#1521);
#1261=LINE('',#6424,#1522);
#1262=LINE('',#6426,#1523);
#1263=LINE('',#6427,#1524);
#1264=LINE('',#6429,#1525);
#1265=LINE('',#6431,#1526);
#1266=LINE('',#6442,#1527);
#1267=LINE('',#6448,#1528);
#1268=LINE('',#6452,#1529);
#1269=LINE('',#6464,#1530);
#1270=LINE('',#6470,#1531);
#1271=LINE('',#6474,#1532);
#1272=LINE('',#6486,#1533);
#1273=LINE('',#6492,#1534);
#1274=LINE('',#6496,#1535);
#1275=LINE('',#6508,#1536);
#1276=LINE('',#6514,#1537);
#1277=LINE('',#6518,#1538);
#1278=LINE('',#6532,#1539);
#1279=LINE('',#6537,#1540);
#1280=LINE('',#6539,#1541);
#1281=LINE('',#6541,#1542);
#1282=LINE('',#6542,#1543);
#1283=LINE('',#6545,#1544);
#1284=LINE('',#6547,#1545);
#1285=LINE('',#6548,#1546);
#1286=LINE('',#6552,#1547);
#1287=LINE('',#6553,#1548);
#1288=LINE('',#6554,#1549);
#1289=LINE('',#6564,#1550);
#1290=LINE('',#6572,#1551);
#1291=VECTOR('',#4339,0.164999999999999);
#1292=VECTOR('',#4346,0.164999999999999);
#1293=VECTOR('',#4353,0.21);
#1294=VECTOR('',#4360,0.21);
#1295=VECTOR('',#4367,0.21);
#1296=VECTOR('',#4374,0.21);
#1297=VECTOR('',#4381,0.21);
#1298=VECTOR('',#4388,0.21);
#1299=VECTOR('',#4395,0.21);
#1300=VECTOR('',#4402,0.21);
#1301=VECTOR('',#4409,0.21);
#1302=VECTOR('',#4416,0.21);
#1303=VECTOR('',#4423,0.21);
#1304=VECTOR('',#4430,0.21);
#1305=VECTOR('',#4435,1.);
#1306=VECTOR('',#4436,1.);
#1307=VECTOR('',#4437,1.);
#1308=VECTOR('',#4438,1.);
#1309=VECTOR('',#4441,1.);
#1310=VECTOR('',#4442,1.);
#1311=VECTOR('',#4443,1.);
#1312=VECTOR('',#4446,1.);
#1313=VECTOR('',#4447,1.);
#1314=VECTOR('',#4448,1.);
#1315=VECTOR('',#4451,1.);
#1316=VECTOR('',#4452,1.);
#1317=VECTOR('',#4463,0.800000000000001);
#1318=VECTOR('',#4476,0.800000000000001);
#1319=VECTOR('',#4489,0.800000000000001);
#1320=VECTOR('',#4502,0.800000000000001);
#1321=VECTOR('',#4515,0.45);
#1322=VECTOR('',#4526,0.45);
#1323=VECTOR('',#4537,0.45);
#1324=VECTOR('',#4548,0.45);
#1325=VECTOR('',#4559,0.275);
#1326=VECTOR('',#4564,0.275);
#1327=VECTOR('',#4569,0.275);
#1328=VECTOR('',#4574,0.275);
#1329=VECTOR('',#4577,1.);
#1330=VECTOR('',#4578,1.);
#1331=VECTOR('',#4579,1.);
#1332=VECTOR('',#4580,1.);
#1333=VECTOR('',#4583,1.);
#1334=VECTOR('',#4584,1.);
#1335=VECTOR('',#4585,1.);
#1336=VECTOR('',#4588,1.);
#1337=VECTOR('',#4589,1.);
#1338=VECTOR('',#4590,1.);
#1339=VECTOR('',#4593,1.);
#1340=VECTOR('',#4594,1.);
#1341=VECTOR('',#4599,1.);
#1342=VECTOR('',#4600,1.);
#1343=VECTOR('',#4601,1.);
#1344=VECTOR('',#4602,1.);
#1345=VECTOR('',#4605,1.);
#1346=VECTOR('',#4606,1.);
#1347=VECTOR('',#4607,1.);
#1348=VECTOR('',#4610,1.);
#1349=VECTOR('',#4611,1.);
#1350=VECTOR('',#4612,1.);
#1351=VECTOR('',#4615,1.);
#1352=VECTOR('',#4616,1.);
#1353=VECTOR('',#4625,1.);
#1354=VECTOR('',#4626,1.);
#1355=VECTOR('',#4627,1.);
#1356=VECTOR('',#4628,1.);
#1357=VECTOR('',#4631,1.);
#1358=VECTOR('',#4632,1.);
#1359=VECTOR('',#4633,1.);
#1360=VECTOR('',#4636,1.);
#1361=VECTOR('',#4637,1.);
#1362=VECTOR('',#4638,1.);
#1363=VECTOR('',#4641,1.);
#1364=VECTOR('',#4642,1.);
#1365=VECTOR('',#4653,0.475);
#1366=VECTOR('',#4664,0.275);
#1367=VECTOR('',#4669,0.275);
#1368=VECTOR('',#4676,0.405);
#1369=VECTOR('',#4681,1.);
#1370=VECTOR('',#4682,1.);
#1371=VECTOR('',#4683,1.);
#1372=VECTOR('',#4684,1.);
#1373=VECTOR('',#4687,1.);
#1374=VECTOR('',#4688,1.);
#1375=VECTOR('',#4689,1.);
#1376=VECTOR('',#4692,1.);
#1377=VECTOR('',#4693,1.);
#1378=VECTOR('',#4694,1.);
#1379=VECTOR('',#4697,1.);
#1380=VECTOR('',#4698,1.);
#1381=VECTOR('',#4699,1.);
#1382=VECTOR('',#4702,1.);
#1383=VECTOR('',#4703,1.);
#1384=VECTOR('',#4704,1.);
#1385=VECTOR('',#4707,1.);
#1386=VECTOR('',#4708,1.);
#1387=VECTOR('',#4719,0.475);
#1388=VECTOR('',#4730,0.275);
#1389=VECTOR('',#4735,0.275);
#1390=VECTOR('',#4742,0.405);
#1391=VECTOR('',#4747,1.);
#1392=VECTOR('',#4748,1.);
#1393=VECTOR('',#4749,1.);
#1394=VECTOR('',#4750,1.);
#1395=VECTOR('',#4753,1.);
#1396=VECTOR('',#4754,1.);
#1397=VECTOR('',#4755,1.);
#1398=VECTOR('',#4758,1.);
#1399=VECTOR('',#4759,1.);
#1400=VECTOR('',#4760,1.);
#1401=VECTOR('',#4763,1.);
#1402=VECTOR('',#4764,1.);
#1403=VECTOR('',#4765,1.);
#1404=VECTOR('',#4768,1.);
#1405=VECTOR('',#4769,1.);
#1406=VECTOR('',#4770,1.);
#1407=VECTOR('',#4773,1.);
#1408=VECTOR('',#4774,1.);
#1409=VECTOR('',#4785,0.165);
#1410=VECTOR('',#4794,0.165);
#1411=VECTOR('',#4803,0.4);
#1412=VECTOR('',#4816,0.225);
#1413=VECTOR('',#4823,0.8);
#1414=VECTOR('',#4836,0.225);
#1415=VECTOR('',#4843,0.8);
#1416=VECTOR('',#4856,0.164999999999999);
#1417=VECTOR('',#4871,0.225);
#1418=VECTOR('',#4874,1.);
#1419=VECTOR('',#4875,1.);
#1420=VECTOR('',#4888,0.225);
#1421=VECTOR('',#4891,1.);
#1422=VECTOR('',#4892,1.);
#1423=VECTOR('',#4899,0.6);
#1424=VECTOR('',#4912,1.2);
#1425=VECTOR('',#4919,0.300000000000001);
#1426=VECTOR('',#4934,0.305);
#1427=VECTOR('',#4941,0.5);
#1428=VECTOR('',#4954,0.225);
#1429=VECTOR('',#4961,0.6);
#1430=VECTOR('',#4972,1.);
#1431=VECTOR('',#4973,1.);
#1432=VECTOR('',#4974,1.);
#1433=VECTOR('',#4975,1.);
#1434=VECTOR('',#4978,1.);
#1435=VECTOR('',#4979,1.);
#1436=VECTOR('',#4980,1.);
#1437=VECTOR('',#4983,1.);
#1438=VECTOR('',#4984,1.);
#1439=VECTOR('',#4985,1.);
#1440=VECTOR('',#4988,1.);
#1441=VECTOR('',#4989,1.);
#1442=VECTOR('',#4990,1.);
#1443=VECTOR('',#4993,1.);
#1444=VECTOR('',#4994,1.);
#1445=VECTOR('',#4995,1.);
#1446=VECTOR('',#4998,1.);
#1447=VECTOR('',#4999,1.);
#1448=VECTOR('',#5016,0.4);
#1449=VECTOR('',#5021,0.425);
#1450=VECTOR('',#5026,0.41);
#1451=VECTOR('',#5035,0.26);
#1452=VECTOR('',#5038,0.25);
#1453=VECTOR('',#5043,1.);
#1454=VECTOR('',#5044,1.);
#1455=VECTOR('',#5045,1.);
#1456=VECTOR('',#5046,1.);
#1457=VECTOR('',#5049,1.);
#1458=VECTOR('',#5050,1.);
#1459=VECTOR('',#5051,1.);
#1460=VECTOR('',#5054,1.);
#1461=VECTOR('',#5055,1.);
#1462=VECTOR('',#5056,1.);
#1463=VECTOR('',#5059,1.);
#1464=VECTOR('',#5060,1.);
#1465=VECTOR('',#5061,1.);
#1466=VECTOR('',#5064,1.);
#1467=VECTOR('',#5065,1.);
#1468=VECTOR('',#5066,1.);
#1469=VECTOR('',#5069,1.);
#1470=VECTOR('',#5070,1.);
#1471=VECTOR('',#5087,0.325);
#1472=VECTOR('',#5092,0.35);
#1473=VECTOR('',#5097,0.335);
#1474=VECTOR('',#5106,0.21);
#1475=VECTOR('',#5109,0.2);
#1476=VECTOR('',#5174,0.7);
#1477=VECTOR('',#5181,0.7);
#1478=VECTOR('',#5188,0.6);
#1479=VECTOR('',#5195,0.6);
#1480=VECTOR('',#5202,1.);
#1481=VECTOR('',#5203,1.);
#1482=VECTOR('',#5204,1.);
#1483=VECTOR('',#5209,1.);
#1484=VECTOR('',#5210,1.);
#1485=VECTOR('',#5211,1.);
#1486=VECTOR('',#5216,1.);
#1487=VECTOR('',#5217,1.);
#1488=VECTOR('',#5222,0.405);
#1489=VECTOR('',#5225,1.);
#1490=VECTOR('',#5228,1.);
#1491=VECTOR('',#5229,1.);
#1492=VECTOR('',#5230,1.);
#1493=VECTOR('',#5231,1.);
#1494=VECTOR('',#5232,1.);
#1495=VECTOR('',#5235,1.);
#1496=VECTOR('',#5236,1.);
#1497=VECTOR('',#5237,1.);
#1498=VECTOR('',#5240,1.);
#1499=VECTOR('',#5241,1.);
#1500=VECTOR('',#5242,1.);
#1501=VECTOR('',#5245,1.);
#1502=VECTOR('',#5246,1.);
#1503=VECTOR('',#5247,1.);
#1504=VECTOR('',#5250,1.);
#1505=VECTOR('',#5251,1.);
#1506=VECTOR('',#5252,1.);
#1507=VECTOR('',#5253,1.);
#1508=VECTOR('',#5254,1.);
#1509=VECTOR('',#5255,1.);
#1510=VECTOR('',#5256,1.);
#1511=VECTOR('',#5257,1.);
#1512=VECTOR('',#5260,1.);
#1513=VECTOR('',#5261,1.);
#1514=VECTOR('',#5264,1.);
#1515=VECTOR('',#5265,1.);
#1516=VECTOR('',#5268,1.);
#1517=VECTOR('',#5269,1.);
#1518=VECTOR('',#5272,1.);
#1519=VECTOR('',#5273,1.);
#1520=VECTOR('',#5276,1.);
#1521=VECTOR('',#5277,1.);
#1522=VECTOR('',#5280,1.);
#1523=VECTOR('',#5281,1.);
#1524=VECTOR('',#5282,1.);
#1525=VECTOR('',#5285,1.);
#1526=VECTOR('',#5288,1.);
#1527=VECTOR('',#5303,0.8);
#1528=VECTOR('',#5310,0.4);
#1529=VECTOR('',#5315,0.6);
#1530=VECTOR('',#5332,0.8);
#1531=VECTOR('',#5339,0.4);
#1532=VECTOR('',#5344,0.6);
#1533=VECTOR('',#5361,0.9);
#1534=VECTOR('',#5368,0.5);
#1535=VECTOR('',#5373,0.7);
#1536=VECTOR('',#5390,0.9);
#1537=VECTOR('',#5397,0.5);
#1538=VECTOR('',#5402,0.7);
#1539=VECTOR('',#5425,0.305);
#1540=VECTOR('',#5430,1.);
#1541=VECTOR('',#5431,1.);
#1542=VECTOR('',#5432,1.);
#1543=VECTOR('',#5433,1.);
#1544=VECTOR('',#5436,1.);
#1545=VECTOR('',#5437,1.);
#1546=VECTOR('',#5438,1.);
#1547=VECTOR('',#5441,1.);
#1548=VECTOR('',#5442,1.);
#1549=VECTOR('',#5443,1.);
#1550=VECTOR('',#5458,1.);
#1551=VECTOR('',#5469,0.6);
#1552=CIRCLE('',#3885,0.164999999999999);
#1553=CIRCLE('',#3886,0.164999999999999);
#1554=CIRCLE('',#3888,0.164999999999999);
#1555=CIRCLE('',#3889,0.164999999999999);
#1556=CIRCLE('',#3891,0.21);
#1557=CIRCLE('',#3892,0.21);
#1558=CIRCLE('',#3894,0.21);
#1559=CIRCLE('',#3895,0.21);
#1560=CIRCLE('',#3897,0.21);
#1561=CIRCLE('',#3898,0.21);
#1562=CIRCLE('',#3900,0.21);
#1563=CIRCLE('',#3901,0.21);
#1564=CIRCLE('',#3903,0.21);
#1565=CIRCLE('',#3904,0.21);
#1566=CIRCLE('',#3906,0.21);
#1567=CIRCLE('',#3907,0.21);
#1568=CIRCLE('',#3909,0.21);
#1569=CIRCLE('',#3910,0.21);
#1570=CIRCLE('',#3912,0.21);
#1571=CIRCLE('',#3913,0.21);
#1572=CIRCLE('',#3915,0.21);
#1573=CIRCLE('',#3916,0.21);
#1574=CIRCLE('',#3918,0.21);
#1575=CIRCLE('',#3919,0.21);
#1576=CIRCLE('',#3921,0.21);
#1577=CIRCLE('',#3922,0.21);
#1578=CIRCLE('',#3924,0.21);
#1579=CIRCLE('',#3925,0.21);
#1580=CIRCLE('',#3934,0.800000000000001);
#1581=CIRCLE('',#3935,0.800000000000001);
#1582=CIRCLE('',#3940,0.800000000000001);
#1583=CIRCLE('',#3941,0.800000000000001);
#1584=CIRCLE('',#3946,0.800000000000001);
#1585=CIRCLE('',#3947,0.800000000000001);
#1586=CIRCLE('',#3952,0.800000000000001);
#1587=CIRCLE('',#3953,0.800000000000001);
#1588=CIRCLE('',#3958,0.45);
#1589=CIRCLE('',#3959,0.45);
#1590=CIRCLE('',#3961,0.275);
#1591=CIRCLE('',#3963,0.45);
#1592=CIRCLE('',#3964,0.45);
#1593=CIRCLE('',#3966,0.275);
#1594=CIRCLE('',#3968,0.45);
#1595=CIRCLE('',#3969,0.45);
#1596=CIRCLE('',#3971,0.275);
#1597=CIRCLE('',#3973,0.45);
#1598=CIRCLE('',#3974,0.45);
#1599=CIRCLE('',#3976,0.275);
#1600=CIRCLE('',#3978,0.275);
#1601=CIRCLE('',#3980,0.275);
#1602=CIRCLE('',#3982,0.275);
#1603=CIRCLE('',#3984,0.275);
#1604=CIRCLE('',#4005,0.475);
#1605=CIRCLE('',#4006,0.475);
#1606=CIRCLE('',#4008,0.275);
#1607=CIRCLE('',#4010,0.275);
#1608=CIRCLE('',#4012,0.275);
#1609=CIRCLE('',#4013,0.275);
#1610=CIRCLE('',#4015,0.405);
#1611=CIRCLE('',#4016,0.405);
#1612=CIRCLE('',#4027,0.475);
#1613=CIRCLE('',#4028,0.475);
#1614=CIRCLE('',#4030,0.275);
#1615=CIRCLE('',#4032,0.275);
#1616=CIRCLE('',#4034,0.275);
#1617=CIRCLE('',#4035,0.275);
#1618=CIRCLE('',#4037,0.405);
#1619=CIRCLE('',#4038,0.405);
#1620=CIRCLE('',#4049,0.165);
#1621=CIRCLE('',#4050,0.165);
#1622=CIRCLE('',#4053,0.165);
#1623=CIRCLE('',#4054,0.165);
#1624=CIRCLE('',#4057,0.4);
#1625=CIRCLE('',#4058,0.4);
#1626=CIRCLE('',#4063,0.225);
#1627=CIRCLE('',#4064,0.225);
#1628=CIRCLE('',#4066,0.8);
#1629=CIRCLE('',#4067,0.8);
#1630=CIRCLE('',#4072,0.225);
#1631=CIRCLE('',#4073,0.225);
#1632=CIRCLE('',#4075,0.8);
#1633=CIRCLE('',#4076,0.8);
#1634=CIRCLE('',#4081,0.164999999999999);
#1635=CIRCLE('',#4082,0.164999999999999);
#1636=CIRCLE('',#4085,0.6);
#1637=CIRCLE('',#4086,0.225);
#1638=CIRCLE('',#4088,0.225);
#1639=CIRCLE('',#4089,0.225);
#1640=CIRCLE('',#4090,0.225);
#1641=CIRCLE('',#4092,0.6);
#1642=CIRCLE('',#4093,0.225);
#1643=CIRCLE('',#4095,0.225);
#1644=CIRCLE('',#4096,0.225);
#1645=CIRCLE('',#4097,0.225);
#1646=CIRCLE('',#4099,0.6);
#1647=CIRCLE('',#4100,0.6);
#1648=CIRCLE('',#4101,0.6);
#1649=CIRCLE('',#4102,0.6);
#1650=CIRCLE('',#4104,1.2);
#1651=CIRCLE('',#4106,1.2);
#1652=CIRCLE('',#4108,0.300000000000001);
#1653=CIRCLE('',#4109,0.300000000000001);
#1654=CIRCLE('',#4115,0.305);
#1655=CIRCLE('',#4116,0.305);
#1656=CIRCLE('',#4118,0.5);
#1657=CIRCLE('',#4119,0.5);
#1658=CIRCLE('',#4124,0.225);
#1659=CIRCLE('',#4125,0.225);
#1660=CIRCLE('',#4127,0.6);
#1661=CIRCLE('',#4128,0.6);
#1662=CIRCLE('',#4141,0.24505);
#1663=CIRCLE('',#4143,0.375);
#1664=CIRCLE('',#4145,0.425);
#1665=CIRCLE('',#4147,0.425);
#1666=CIRCLE('',#4149,0.395);
#1667=CIRCLE('',#4151,0.27);
#1668=CIRCLE('',#4153,0.24505);
#1669=CIRCLE('',#4165,0.1954);
#1670=CIRCLE('',#4167,0.3);
#1671=CIRCLE('',#4169,0.35);
#1672=CIRCLE('',#4171,0.35);
#1673=CIRCLE('',#4173,0.32);
#1674=CIRCLE('',#4175,0.22);
#1675=CIRCLE('',#4177,0.1954);
#1676=CIRCLE('',#4210,0.7);
#1677=CIRCLE('',#4211,0.7);
#1678=CIRCLE('',#4213,0.7);
#1679=CIRCLE('',#4214,0.7);
#1680=CIRCLE('',#4216,0.6);
#1681=CIRCLE('',#4217,0.6);
#1682=CIRCLE('',#4219,0.6);
#1683=CIRCLE('',#4220,0.6);
#1684=CIRCLE('',#4222,0.8);
#1685=CIRCLE('',#4223,0.405);
#1686=CIRCLE('',#4226,0.8);
#1687=CIRCLE('',#4227,0.405);
#1688=CIRCLE('',#4246,0.8);
#1689=CIRCLE('',#4247,0.6);
#1690=CIRCLE('',#4249,0.8);
#1691=CIRCLE('',#4251,0.4);
#1692=CIRCLE('',#4253,0.4);
#1693=CIRCLE('',#4255,0.6);
#1694=CIRCLE('',#4259,0.8);
#1695=CIRCLE('',#4260,0.6);
#1696=CIRCLE('',#4262,0.8);
#1697=CIRCLE('',#4264,0.4);
#1698=CIRCLE('',#4266,0.4);
#1699=CIRCLE('',#4268,0.6);
#1700=CIRCLE('',#4272,0.9);
#1701=CIRCLE('',#4273,0.7);
#1702=CIRCLE('',#4275,0.9);
#1703=CIRCLE('',#4277,0.5);
#1704=CIRCLE('',#4279,0.5);
#1705=CIRCLE('',#4281,0.7);
#1706=CIRCLE('',#4285,0.9);
#1707=CIRCLE('',#4286,0.7);
#1708=CIRCLE('',#4288,0.9);
#1709=CIRCLE('',#4290,0.5);
#1710=CIRCLE('',#4292,0.5);
#1711=CIRCLE('',#4294,0.7);
#1712=CIRCLE('',#4304,0.305);
#1713=CIRCLE('',#4305,0.305);
#1714=CIRCLE('',#4310,1.4);
#1715=CIRCLE('',#4312,1.4);
#1716=CIRCLE('',#4313,1.);
#1717=CIRCLE('',#4316,1.);
#1718=CIRCLE('',#4320,0.6);
#1719=CIRCLE('',#4321,0.6);
#1720=VERTEX_POINT('',#5490);
#1721=VERTEX_POINT('',#5492);
#1722=VERTEX_POINT('',#5496);
#1723=VERTEX_POINT('',#5498);
#1724=VERTEX_POINT('',#5502);
#1725=VERTEX_POINT('',#5504);
#1726=VERTEX_POINT('',#5508);
#1727=VERTEX_POINT('',#5510);
#1728=VERTEX_POINT('',#5514);
#1729=VERTEX_POINT('',#5516);
#1730=VERTEX_POINT('',#5520);
#1731=VERTEX_POINT('',#5522);
#1732=VERTEX_POINT('',#5526);
#1733=VERTEX_POINT('',#5528);
#1734=VERTEX_POINT('',#5532);
#1735=VERTEX_POINT('',#5534);
#1736=VERTEX_POINT('',#5538);
#1737=VERTEX_POINT('',#5540);
#1738=VERTEX_POINT('',#5544);
#1739=VERTEX_POINT('',#5546);
#1740=VERTEX_POINT('',#5550);
#1741=VERTEX_POINT('',#5552);
#1742=VERTEX_POINT('',#5556);
#1743=VERTEX_POINT('',#5558);
#1744=VERTEX_POINT('',#5562);
#1745=VERTEX_POINT('',#5564);
#1746=VERTEX_POINT('',#5568);
#1747=VERTEX_POINT('',#5570);
#1748=VERTEX_POINT('',#5574);
#1749=VERTEX_POINT('',#5575);
#1750=VERTEX_POINT('',#5577);
#1751=VERTEX_POINT('',#5579);
#1752=VERTEX_POINT('',#5583);
#1753=VERTEX_POINT('',#5585);
#1754=VERTEX_POINT('',#5589);
#1755=VERTEX_POINT('',#5591);
#1756=VERTEX_POINT('',#5601);
#1757=VERTEX_POINT('',#5603);
#1758=VERTEX_POINT('',#5610);
#1759=VERTEX_POINT('',#5612);
#1760=VERTEX_POINT('',#5619);
#1761=VERTEX_POINT('',#5621);
#1762=VERTEX_POINT('',#5628);
#1763=VERTEX_POINT('',#5630);
#1764=VERTEX_POINT('',#5637);
#1765=VERTEX_POINT('',#5639);
#1766=VERTEX_POINT('',#5643);
#1767=VERTEX_POINT('',#5646);
#1768=VERTEX_POINT('',#5648);
#1769=VERTEX_POINT('',#5652);
#1770=VERTEX_POINT('',#5655);
#1771=VERTEX_POINT('',#5657);
#1772=VERTEX_POINT('',#5661);
#1773=VERTEX_POINT('',#5664);
#1774=VERTEX_POINT('',#5666);
#1775=VERTEX_POINT('',#5670);
#1776=VERTEX_POINT('',#5673);
#1777=VERTEX_POINT('',#5677);
#1778=VERTEX_POINT('',#5681);
#1779=VERTEX_POINT('',#5685);
#1780=VERTEX_POINT('',#5689);
#1781=VERTEX_POINT('',#5690);
#1782=VERTEX_POINT('',#5692);
#1783=VERTEX_POINT('',#5694);
#1784=VERTEX_POINT('',#5698);
#1785=VERTEX_POINT('',#5700);
#1786=VERTEX_POINT('',#5704);
#1787=VERTEX_POINT('',#5706);
#1788=VERTEX_POINT('',#5714);
#1789=VERTEX_POINT('',#5715);
#1790=VERTEX_POINT('',#5717);
#1791=VERTEX_POINT('',#5719);
#1792=VERTEX_POINT('',#5723);
#1793=VERTEX_POINT('',#5725);
#1794=VERTEX_POINT('',#5729);
#1795=VERTEX_POINT('',#5731);
#1796=VERTEX_POINT('',#5741);
#1797=VERTEX_POINT('',#5742);
#1798=VERTEX_POINT('',#5744);
#1799=VERTEX_POINT('',#5746);
#1800=VERTEX_POINT('',#5750);
#1801=VERTEX_POINT('',#5752);
#1802=VERTEX_POINT('',#5756);
#1803=VERTEX_POINT('',#5758);
#1804=VERTEX_POINT('',#5768);
#1805=VERTEX_POINT('',#5770);
#1806=VERTEX_POINT('',#5773);
#1807=VERTEX_POINT('',#5825);
#1808=VERTEX_POINT('',#5828);
#1809=VERTEX_POINT('',#5832);
#1810=VERTEX_POINT('',#5834);
#1811=VERTEX_POINT('',#5838);
#1812=VERTEX_POINT('',#5840);
#1813=VERTEX_POINT('',#5844);
#1814=VERTEX_POINT('',#5845);
#1815=VERTEX_POINT('',#5847);
#1816=VERTEX_POINT('',#5849);
#1817=VERTEX_POINT('',#5853);
#1818=VERTEX_POINT('',#5855);
#1819=VERTEX_POINT('',#5859);
#1820=VERTEX_POINT('',#5861);
#1821=VERTEX_POINT('',#5865);
#1822=VERTEX_POINT('',#5867);
#1823=VERTEX_POINT('',#5871);
#1824=VERTEX_POINT('',#5873);
#1825=VERTEX_POINT('',#5883);
#1826=VERTEX_POINT('',#5885);
#1827=VERTEX_POINT('',#5888);
#1828=VERTEX_POINT('',#5940);
#1829=VERTEX_POINT('',#5943);
#1830=VERTEX_POINT('',#5947);
#1831=VERTEX_POINT('',#5949);
#1832=VERTEX_POINT('',#5953);
#1833=VERTEX_POINT('',#5955);
#1834=VERTEX_POINT('',#5959);
#1835=VERTEX_POINT('',#5960);
#1836=VERTEX_POINT('',#5962);
#1837=VERTEX_POINT('',#5964);
#1838=VERTEX_POINT('',#5968);
#1839=VERTEX_POINT('',#5970);
#1840=VERTEX_POINT('',#5974);
#1841=VERTEX_POINT('',#5976);
#1842=VERTEX_POINT('',#5980);
#1843=VERTEX_POINT('',#5982);
#1844=VERTEX_POINT('',#5986);
#1845=VERTEX_POINT('',#5988);
#1846=VERTEX_POINT('',#5998);
#1847=VERTEX_POINT('',#6000);
#1848=VERTEX_POINT('',#6005);
#1849=VERTEX_POINT('',#6007);
#1850=VERTEX_POINT('',#6012);
#1851=VERTEX_POINT('',#6014);
#1852=VERTEX_POINT('',#6021);
#1853=VERTEX_POINT('',#6023);
#1854=VERTEX_POINT('',#6027);
#1855=VERTEX_POINT('',#6029);
#1856=VERTEX_POINT('',#6036);
#1857=VERTEX_POINT('',#6038);
#1858=VERTEX_POINT('',#6042);
#1859=VERTEX_POINT('',#6044);
#1860=VERTEX_POINT('',#6051);
#1861=VERTEX_POINT('',#6053);
#1862=VERTEX_POINT('',#6058);
#1863=VERTEX_POINT('',#6059);
#1864=VERTEX_POINT('',#6063);
#1865=VERTEX_POINT('',#6065);
#1866=VERTEX_POINT('',#6067);
#1867=VERTEX_POINT('',#6070);
#1868=VERTEX_POINT('',#6074);
#1869=VERTEX_POINT('',#6075);
#1870=VERTEX_POINT('',#6079);
#1871=VERTEX_POINT('',#6081);
#1872=VERTEX_POINT('',#6083);
#1873=VERTEX_POINT('',#6086);
#1874=VERTEX_POINT('',#6090);
#1875=VERTEX_POINT('',#6092);
#1876=VERTEX_POINT('',#6098);
#1877=VERTEX_POINT('',#6101);
#1878=VERTEX_POINT('',#6105);
#1879=VERTEX_POINT('',#6107);
#1880=VERTEX_POINT('',#6115);
#1881=VERTEX_POINT('',#6117);
#1882=VERTEX_POINT('',#6121);
#1883=VERTEX_POINT('',#6123);
#1884=VERTEX_POINT('',#6130);
#1885=VERTEX_POINT('',#6132);
#1886=VERTEX_POINT('',#6136);
#1887=VERTEX_POINT('',#6138);
#1888=VERTEX_POINT('',#6145);
#1889=VERTEX_POINT('',#6146);
#1890=VERTEX_POINT('',#6148);
#1891=VERTEX_POINT('',#6150);
#1892=VERTEX_POINT('',#6154);
#1893=VERTEX_POINT('',#6156);
#1894=VERTEX_POINT('',#6160);
#1895=VERTEX_POINT('',#6162);
#1896=VERTEX_POINT('',#6166);
#1897=VERTEX_POINT('',#6168);
#1898=VERTEX_POINT('',#6172);
#1899=VERTEX_POINT('',#6174);
#1900=VERTEX_POINT('',#6183);
#1901=VERTEX_POINT('',#6186);
#1902=VERTEX_POINT('',#6189);
#1903=VERTEX_POINT('',#6193);
#1904=VERTEX_POINT('',#6197);
#1905=VERTEX_POINT('',#6201);
#1906=VERTEX_POINT('',#6204);
#1907=VERTEX_POINT('',#6211);
#1908=VERTEX_POINT('',#6212);
#1909=VERTEX_POINT('',#6214);
#1910=VERTEX_POINT('',#6216);
#1911=VERTEX_POINT('',#6220);
#1912=VERTEX_POINT('',#6222);
#1913=VERTEX_POINT('',#6226);
#1914=VERTEX_POINT('',#6228);
#1915=VERTEX_POINT('',#6232);
#1916=VERTEX_POINT('',#6234);
#1917=VERTEX_POINT('',#6238);
#1918=VERTEX_POINT('',#6240);
#1919=VERTEX_POINT('',#6249);
#1920=VERTEX_POINT('',#6252);
#1921=VERTEX_POINT('',#6255);
#1922=VERTEX_POINT('',#6259);
#1923=VERTEX_POINT('',#6263);
#1924=VERTEX_POINT('',#6267);
#1925=VERTEX_POINT('',#6270);
#1926=VERTEX_POINT('',#6306);
#1927=VERTEX_POINT('',#6308);
#1928=VERTEX_POINT('',#6312);
#1929=VERTEX_POINT('',#6314);
#1930=VERTEX_POINT('',#6318);
#1931=VERTEX_POINT('',#6320);
#1932=VERTEX_POINT('',#6324);
#1933=VERTEX_POINT('',#6326);
#1934=VERTEX_POINT('',#6330);
#1935=VERTEX_POINT('',#6331);
#1936=VERTEX_POINT('',#6333);
#1937=VERTEX_POINT('',#6335);
#1938=VERTEX_POINT('',#6338);
#1939=VERTEX_POINT('',#6341);
#1940=VERTEX_POINT('',#6343);
#1941=VERTEX_POINT('',#6347);
#1942=VERTEX_POINT('',#6349);
#1943=VERTEX_POINT('',#6352);
#1944=VERTEX_POINT('',#6359);
#1945=VERTEX_POINT('',#6361);
#1946=VERTEX_POINT('',#6363);
#1947=VERTEX_POINT('',#6365);
#1948=VERTEX_POINT('',#6369);
#1949=VERTEX_POINT('',#6371);
#1950=VERTEX_POINT('',#6375);
#1951=VERTEX_POINT('',#6377);
#1952=VERTEX_POINT('',#6381);
#1953=VERTEX_POINT('',#6383);
#1954=VERTEX_POINT('',#6387);
#1955=VERTEX_POINT('',#6389);
#1956=VERTEX_POINT('',#6391);
#1957=VERTEX_POINT('',#6393);
#1958=VERTEX_POINT('',#6395);
#1959=VERTEX_POINT('',#6397);
#1960=VERTEX_POINT('',#6399);
#1961=VERTEX_POINT('',#6403);
#1962=VERTEX_POINT('',#6407);
#1963=VERTEX_POINT('',#6411);
#1964=VERTEX_POINT('',#6415);
#1965=VERTEX_POINT('',#6419);
#1966=VERTEX_POINT('',#6423);
#1967=VERTEX_POINT('',#6425);
#1968=VERTEX_POINT('',#6435);
#1969=VERTEX_POINT('',#6437);
#1970=VERTEX_POINT('',#6440);
#1971=VERTEX_POINT('',#6444);
#1972=VERTEX_POINT('',#6447);
#1973=VERTEX_POINT('',#6451);
#1974=VERTEX_POINT('',#6457);
#1975=VERTEX_POINT('',#6459);
#1976=VERTEX_POINT('',#6462);
#1977=VERTEX_POINT('',#6466);
#1978=VERTEX_POINT('',#6469);
#1979=VERTEX_POINT('',#6473);
#1980=VERTEX_POINT('',#6479);
#1981=VERTEX_POINT('',#6481);
#1982=VERTEX_POINT('',#6484);
#1983=VERTEX_POINT('',#6488);
#1984=VERTEX_POINT('',#6491);
#1985=VERTEX_POINT('',#6495);
#1986=VERTEX_POINT('',#6501);
#1987=VERTEX_POINT('',#6503);
#1988=VERTEX_POINT('',#6506);
#1989=VERTEX_POINT('',#6510);
#1990=VERTEX_POINT('',#6513);
#1991=VERTEX_POINT('',#6517);
#1992=VERTEX_POINT('',#6529);
#1993=VERTEX_POINT('',#6531);
#1994=VERTEX_POINT('',#6535);
#1995=VERTEX_POINT('',#6536);
#1996=VERTEX_POINT('',#6538);
#1997=VERTEX_POINT('',#6540);
#1998=VERTEX_POINT('',#6544);
#1999=VERTEX_POINT('',#6546);
#2000=VERTEX_POINT('',#6550);
#2001=VERTEX_POINT('',#6551);
#2002=VERTEX_POINT('',#6559);
#2003=VERTEX_POINT('',#6563);
#2004=VERTEX_POINT('',#6569);
#2005=VERTEX_POINT('',#6571);
#2006=EDGE_CURVE('',#1720,#1720,#1552,.T.);
#2007=EDGE_CURVE('',#1720,#1721,#1030,.T.);
#2008=EDGE_CURVE('',#1721,#1721,#1553,.T.);
#2009=EDGE_CURVE('',#1722,#1722,#1554,.T.);
#2010=EDGE_CURVE('',#1722,#1723,#1031,.T.);
#2011=EDGE_CURVE('',#1723,#1723,#1555,.T.);
#2012=EDGE_CURVE('',#1724,#1724,#1556,.T.);
#2013=EDGE_CURVE('',#1724,#1725,#1032,.T.);
#2014=EDGE_CURVE('',#1725,#1725,#1557,.T.);
#2015=EDGE_CURVE('',#1726,#1726,#1558,.T.);
#2016=EDGE_CURVE('',#1726,#1727,#1033,.T.);
#2017=EDGE_CURVE('',#1727,#1727,#1559,.T.);
#2018=EDGE_CURVE('',#1728,#1728,#1560,.T.);
#2019=EDGE_CURVE('',#1728,#1729,#1034,.T.);
#2020=EDGE_CURVE('',#1729,#1729,#1561,.T.);
#2021=EDGE_CURVE('',#1730,#1730,#1562,.T.);
#2022=EDGE_CURVE('',#1730,#1731,#1035,.T.);
#2023=EDGE_CURVE('',#1731,#1731,#1563,.T.);
#2024=EDGE_CURVE('',#1732,#1732,#1564,.T.);
#2025=EDGE_CURVE('',#1732,#1733,#1036,.T.);
#2026=EDGE_CURVE('',#1733,#1733,#1565,.T.);
#2027=EDGE_CURVE('',#1734,#1734,#1566,.T.);
#2028=EDGE_CURVE('',#1734,#1735,#1037,.T.);
#2029=EDGE_CURVE('',#1735,#1735,#1567,.T.);
#2030=EDGE_CURVE('',#1736,#1736,#1568,.T.);
#2031=EDGE_CURVE('',#1736,#1737,#1038,.T.);
#2032=EDGE_CURVE('',#1737,#1737,#1569,.T.);
#2033=EDGE_CURVE('',#1738,#1738,#1570,.T.);
#2034=EDGE_CURVE('',#1738,#1739,#1039,.T.);
#2035=EDGE_CURVE('',#1739,#1739,#1571,.T.);
#2036=EDGE_CURVE('',#1740,#1740,#1572,.T.);
#2037=EDGE_CURVE('',#1740,#1741,#1040,.T.);
#2038=EDGE_CURVE('',#1741,#1741,#1573,.T.);
#2039=EDGE_CURVE('',#1742,#1742,#1574,.T.);
#2040=EDGE_CURVE('',#1742,#1743,#1041,.T.);
#2041=EDGE_CURVE('',#1743,#1743,#1575,.T.);
#2042=EDGE_CURVE('',#1744,#1744,#1576,.T.);
#2043=EDGE_CURVE('',#1744,#1745,#1042,.T.);
#2044=EDGE_CURVE('',#1745,#1745,#1577,.T.);
#2045=EDGE_CURVE('',#1746,#1746,#1578,.T.);
#2046=EDGE_CURVE('',#1746,#1747,#1043,.T.);
#2047=EDGE_CURVE('',#1747,#1747,#1579,.T.);
#2048=EDGE_CURVE('',#1748,#1749,#1044,.T.);
#2049=EDGE_CURVE('',#1749,#1750,#1045,.T.);
#2050=EDGE_CURVE('',#1751,#1750,#1046,.T.);
#2051=EDGE_CURVE('',#1748,#1751,#1047,.T.);
#2052=EDGE_CURVE('',#1752,#1748,#1048,.T.);
#2053=EDGE_CURVE('',#1753,#1751,#1049,.T.);
#2054=EDGE_CURVE('',#1752,#1753,#1050,.T.);
#2055=EDGE_CURVE('',#1754,#1752,#1051,.T.);
#2056=EDGE_CURVE('',#1755,#1753,#1052,.T.);
#2057=EDGE_CURVE('',#1754,#1755,#1053,.T.);
#2058=EDGE_CURVE('',#1749,#1754,#1054,.T.);
#2059=EDGE_CURVE('',#1750,#1755,#1055,.T.);
#2060=EDGE_CURVE('',#1756,#1756,#1580,.T.);
#2061=EDGE_CURVE('',#1756,#1757,#1056,.T.);
#2062=EDGE_CURVE('',#1757,#1757,#1581,.T.);
#2063=EDGE_CURVE('',#1758,#1758,#1582,.T.);
#2064=EDGE_CURVE('',#1758,#1759,#1057,.T.);
#2065=EDGE_CURVE('',#1759,#1759,#1583,.T.);
#2066=EDGE_CURVE('',#1760,#1760,#1584,.T.);
#2067=EDGE_CURVE('',#1760,#1761,#1058,.T.);
#2068=EDGE_CURVE('',#1761,#1761,#1585,.T.);
#2069=EDGE_CURVE('',#1762,#1762,#1586,.T.);
#2070=EDGE_CURVE('',#1762,#1763,#1059,.T.);
#2071=EDGE_CURVE('',#1763,#1763,#1587,.T.);
#2072=EDGE_CURVE('',#1764,#1764,#1588,.T.);
#2073=EDGE_CURVE('',#1764,#1765,#1060,.T.);
#2074=EDGE_CURVE('',#1765,#1765,#1589,.T.);
#2075=EDGE_CURVE('',#1766,#1766,#1590,.T.);
#2076=EDGE_CURVE('',#1767,#1767,#1591,.T.);
#2077=EDGE_CURVE('',#1767,#1768,#1061,.T.);
#2078=EDGE_CURVE('',#1768,#1768,#1592,.T.);
#2079=EDGE_CURVE('',#1769,#1769,#1593,.T.);
#2080=EDGE_CURVE('',#1770,#1770,#1594,.T.);
#2081=EDGE_CURVE('',#1770,#1771,#1062,.T.);
#2082=EDGE_CURVE('',#1771,#1771,#1595,.T.);
#2083=EDGE_CURVE('',#1772,#1772,#1596,.T.);
#2084=EDGE_CURVE('',#1773,#1773,#1597,.T.);
#2085=EDGE_CURVE('',#1773,#1774,#1063,.T.);
#2086=EDGE_CURVE('',#1774,#1774,#1598,.T.);
#2087=EDGE_CURVE('',#1775,#1775,#1599,.T.);
#2088=EDGE_CURVE('',#1776,#1776,#1600,.T.);
#2089=EDGE_CURVE('',#1776,#1766,#1064,.T.);
#2090=EDGE_CURVE('',#1777,#1777,#1601,.T.);
#2091=EDGE_CURVE('',#1777,#1769,#1065,.T.);
#2092=EDGE_CURVE('',#1778,#1778,#1602,.T.);
#2093=EDGE_CURVE('',#1778,#1772,#1066,.T.);
#2094=EDGE_CURVE('',#1779,#1779,#1603,.T.);
#2095=EDGE_CURVE('',#1779,#1775,#1067,.T.);
#2096=EDGE_CURVE('',#1780,#1781,#1068,.T.);
#2097=EDGE_CURVE('',#1782,#1780,#1069,.T.);
#2098=EDGE_CURVE('',#1783,#1782,#1070,.T.);
#2099=EDGE_CURVE('',#1783,#1781,#1071,.T.);
#2100=EDGE_CURVE('',#1781,#1784,#1072,.T.);
#2101=EDGE_CURVE('',#1785,#1783,#1073,.T.);
#2102=EDGE_CURVE('',#1785,#1784,#1074,.T.);
#2103=EDGE_CURVE('',#1784,#1786,#1075,.T.);
#2104=EDGE_CURVE('',#1787,#1785,#1076,.T.);
#2105=EDGE_CURVE('',#1787,#1786,#1077,.T.);
#2106=EDGE_CURVE('',#1786,#1780,#1078,.T.);
#2107=EDGE_CURVE('',#1782,#1787,#1079,.T.);
#2108=EDGE_CURVE('',#1788,#1789,#1080,.T.);
#2109=EDGE_CURVE('',#1789,#1790,#1081,.T.);
#2110=EDGE_CURVE('',#1791,#1790,#1082,.T.);
#2111=EDGE_CURVE('',#1788,#1791,#1083,.T.);
#2112=EDGE_CURVE('',#1792,#1788,#1084,.T.);
#2113=EDGE_CURVE('',#1793,#1791,#1085,.T.);
#2114=EDGE_CURVE('',#1792,#1793,#1086,.T.);
#2115=EDGE_CURVE('',#1794,#1792,#1087,.T.);
#2116=EDGE_CURVE('',#1795,#1793,#1088,.T.);
#2117=EDGE_CURVE('',#1794,#1795,#1089,.T.);
#2118=EDGE_CURVE('',#1789,#1794,#1090,.T.);
#2119=EDGE_CURVE('',#1790,#1795,#1091,.T.);
#2120=EDGE_CURVE('',#1796,#1797,#1092,.T.);
#2121=EDGE_CURVE('',#1797,#1798,#1093,.T.);
#2122=EDGE_CURVE('',#1799,#1798,#1094,.T.);
#2123=EDGE_CURVE('',#1796,#1799,#1095,.T.);
#2124=EDGE_CURVE('',#1800,#1796,#1096,.T.);
#2125=EDGE_CURVE('',#1801,#1799,#1097,.T.);
#2126=EDGE_CURVE('',#1800,#1801,#1098,.T.);
#2127=EDGE_CURVE('',#1802,#1800,#1099,.T.);
#2128=EDGE_CURVE('',#1803,#1801,#1100,.T.);
#2129=EDGE_CURVE('',#1802,#1803,#1101,.T.);
#2130=EDGE_CURVE('',#1797,#1802,#1102,.T.);
#2131=EDGE_CURVE('',#1798,#1803,#1103,.T.);
#2132=EDGE_CURVE('',#1804,#1804,#1604,.T.);
#2133=EDGE_CURVE('',#1804,#1805,#1104,.T.);
#2134=EDGE_CURVE('',#1805,#1805,#1605,.T.);
#2135=EDGE_CURVE('',#1806,#1806,#173,.T.);
#2136=EDGE_CURVE('',#1807,#1807,#1606,.T.);
#2137=EDGE_CURVE('',#1808,#1808,#1607,.T.);
#2138=EDGE_CURVE('',#1808,#1807,#1105,.T.);
#2139=EDGE_CURVE('',#1809,#1809,#1608,.T.);
#2140=EDGE_CURVE('',#1809,#1810,#1106,.T.);
#2141=EDGE_CURVE('',#1810,#1810,#1609,.T.);
#2142=EDGE_CURVE('',#1811,#1811,#1610,.T.);
#2143=EDGE_CURVE('',#1811,#1812,#1107,.T.);
#2144=EDGE_CURVE('',#1812,#1812,#1611,.T.);
#2145=EDGE_CURVE('',#1813,#1814,#1108,.T.);
#2146=EDGE_CURVE('',#1814,#1815,#1109,.T.);
#2147=EDGE_CURVE('',#1816,#1815,#1110,.T.);
#2148=EDGE_CURVE('',#1813,#1816,#1111,.T.);
#2149=EDGE_CURVE('',#1817,#1813,#1112,.T.);
#2150=EDGE_CURVE('',#1818,#1816,#1113,.T.);
#2151=EDGE_CURVE('',#1817,#1818,#1114,.T.);
#2152=EDGE_CURVE('',#1819,#1817,#1115,.T.);
#2153=EDGE_CURVE('',#1820,#1818,#1116,.T.);
#2154=EDGE_CURVE('',#1819,#1820,#1117,.T.);
#2155=EDGE_CURVE('',#1821,#1819,#1118,.T.);
#2156=EDGE_CURVE('',#1822,#1820,#1119,.T.);
#2157=EDGE_CURVE('',#1821,#1822,#1120,.T.);
#2158=EDGE_CURVE('',#1823,#1821,#1121,.T.);
#2159=EDGE_CURVE('',#1824,#1822,#1122,.T.);
#2160=EDGE_CURVE('',#1823,#1824,#1123,.T.);
#2161=EDGE_CURVE('',#1814,#1823,#1124,.T.);
#2162=EDGE_CURVE('',#1815,#1824,#1125,.T.);
#2163=EDGE_CURVE('',#1825,#1825,#1612,.T.);
#2164=EDGE_CURVE('',#1825,#1826,#1126,.T.);
#2165=EDGE_CURVE('',#1826,#1826,#1613,.T.);
#2166=EDGE_CURVE('',#1827,#1827,#174,.T.);
#2167=EDGE_CURVE('',#1828,#1828,#1614,.T.);
#2168=EDGE_CURVE('',#1829,#1829,#1615,.T.);
#2169=EDGE_CURVE('',#1829,#1828,#1127,.T.);
#2170=EDGE_CURVE('',#1830,#1830,#1616,.T.);
#2171=EDGE_CURVE('',#1830,#1831,#1128,.T.);
#2172=EDGE_CURVE('',#1831,#1831,#1617,.T.);
#2173=EDGE_CURVE('',#1832,#1832,#1618,.T.);
#2174=EDGE_CURVE('',#1832,#1833,#1129,.T.);
#2175=EDGE_CURVE('',#1833,#1833,#1619,.T.);
#2176=EDGE_CURVE('',#1834,#1835,#1130,.T.);
#2177=EDGE_CURVE('',#1835,#1836,#1131,.T.);
#2178=EDGE_CURVE('',#1837,#1836,#1132,.T.);
#2179=EDGE_CURVE('',#1834,#1837,#1133,.T.);
#2180=EDGE_CURVE('',#1838,#1834,#1134,.T.);
#2181=EDGE_CURVE('',#1839,#1837,#1135,.T.);
#2182=EDGE_CURVE('',#1838,#1839,#1136,.T.);
#2183=EDGE_CURVE('',#1840,#1838,#1137,.T.);
#2184=EDGE_CURVE('',#1841,#1839,#1138,.T.);
#2185=EDGE_CURVE('',#1840,#1841,#1139,.T.);
#2186=EDGE_CURVE('',#1842,#1840,#1140,.T.);
#2187=EDGE_CURVE('',#1843,#1841,#1141,.T.);
#2188=EDGE_CURVE('',#1842,#1843,#1142,.T.);
#2189=EDGE_CURVE('',#1844,#1842,#1143,.T.);
#2190=EDGE_CURVE('',#1845,#1843,#1144,.T.);
#2191=EDGE_CURVE('',#1844,#1845,#1145,.T.);
#2192=EDGE_CURVE('',#1835,#1844,#1146,.T.);
#2193=EDGE_CURVE('',#1836,#1845,#1147,.T.);
#2194=EDGE_CURVE('',#1846,#1846,#1620,.T.);
#2195=EDGE_CURVE('',#1846,#1847,#1148,.T.);
#2196=EDGE_CURVE('',#1847,#1847,#1621,.T.);
#2197=EDGE_CURVE('',#1848,#1848,#1622,.T.);
#2198=EDGE_CURVE('',#1848,#1849,#1149,.T.);
#2199=EDGE_CURVE('',#1849,#1849,#1623,.T.);
#2200=EDGE_CURVE('',#1850,#1850,#1624,.T.);
#2201=EDGE_CURVE('',#1850,#1851,#1150,.T.);
#2202=EDGE_CURVE('',#1851,#1851,#1625,.T.);
#2203=EDGE_CURVE('',#1852,#1852,#1626,.T.);
#2204=EDGE_CURVE('',#1852,#1853,#1151,.T.);
#2205=EDGE_CURVE('',#1853,#1853,#1627,.T.);
#2206=EDGE_CURVE('',#1854,#1854,#1628,.T.);
#2207=EDGE_CURVE('',#1854,#1855,#1152,.T.);
#2208=EDGE_CURVE('',#1855,#1855,#1629,.T.);
#2209=EDGE_CURVE('',#1856,#1856,#1630,.T.);
#2210=EDGE_CURVE('',#1856,#1857,#1153,.T.);
#2211=EDGE_CURVE('',#1857,#1857,#1631,.T.);
#2212=EDGE_CURVE('',#1858,#1858,#1632,.T.);
#2213=EDGE_CURVE('',#1858,#1859,#1154,.T.);
#2214=EDGE_CURVE('',#1859,#1859,#1633,.T.);
#2215=EDGE_CURVE('',#1860,#1860,#1634,.T.);
#2216=EDGE_CURVE('',#1860,#1861,#1155,.T.);
#2217=EDGE_CURVE('',#1861,#1861,#1635,.T.);
#2218=EDGE_CURVE('',#1862,#1863,#1636,.T.);
#2219=EDGE_CURVE('',#1863,#1862,#1637,.T.);
#2220=EDGE_CURVE('',#1864,#1864,#1638,.T.);
#2221=EDGE_CURVE('',#1864,#1865,#1156,.T.);
#2222=EDGE_CURVE('',#1866,#1865,#1639,.T.);
#2223=EDGE_CURVE('',#1863,#1866,#1157,.T.);
#2224=EDGE_CURVE('',#1867,#1862,#1158,.T.);
#2225=EDGE_CURVE('',#1865,#1867,#1640,.T.);
#2226=EDGE_CURVE('',#1868,#1869,#1641,.T.);
#2227=EDGE_CURVE('',#1869,#1868,#1642,.T.);
#2228=EDGE_CURVE('',#1870,#1870,#1643,.T.);
#2229=EDGE_CURVE('',#1870,#1871,#1159,.T.);
#2230=EDGE_CURVE('',#1872,#1871,#1644,.T.);
#2231=EDGE_CURVE('',#1869,#1872,#1160,.T.);
#2232=EDGE_CURVE('',#1873,#1868,#1161,.T.);
#2233=EDGE_CURVE('',#1871,#1873,#1645,.T.);
#2234=EDGE_CURVE('',#1874,#1874,#1646,.T.);
#2235=EDGE_CURVE('',#1874,#1875,#1162,.T.);
#2236=EDGE_CURVE('',#1875,#1867,#1647,.T.);
#2237=EDGE_CURVE('',#1866,#1873,#1648,.T.);
#2238=EDGE_CURVE('',#1872,#1875,#1649,.T.);
#2239=EDGE_CURVE('',#1876,#1876,#1650,.T.);
#2240=EDGE_CURVE('',#1876,#1877,#1163,.T.);
#2241=EDGE_CURVE('',#1877,#1877,#1651,.T.);
#2242=EDGE_CURVE('',#1878,#1878,#1652,.T.);
#2243=EDGE_CURVE('',#1878,#1879,#1164,.T.);
#2244=EDGE_CURVE('',#1879,#1879,#1653,.T.);
#2245=EDGE_CURVE('',#1880,#1880,#1654,.T.);
#2246=EDGE_CURVE('',#1880,#1881,#1165,.T.);
#2247=EDGE_CURVE('',#1881,#1881,#1655,.T.);
#2248=EDGE_CURVE('',#1882,#1882,#1656,.T.);
#2249=EDGE_CURVE('',#1882,#1883,#1166,.T.);
#2250=EDGE_CURVE('',#1883,#1883,#1657,.T.);
#2251=EDGE_CURVE('',#1884,#1884,#1658,.T.);
#2252=EDGE_CURVE('',#1884,#1885,#1167,.T.);
#2253=EDGE_CURVE('',#1885,#1885,#1659,.T.);
#2254=EDGE_CURVE('',#1886,#1886,#1660,.T.);
#2255=EDGE_CURVE('',#1886,#1887,#1168,.T.);
#2256=EDGE_CURVE('',#1887,#1887,#1661,.T.);
#2257=EDGE_CURVE('',#1888,#1889,#1169,.T.);
#2258=EDGE_CURVE('',#1889,#1890,#1170,.T.);
#2259=EDGE_CURVE('',#1890,#1891,#1171,.T.);
#2260=EDGE_CURVE('',#1888,#1891,#1172,.T.);
#2261=EDGE_CURVE('',#1889,#1892,#1173,.T.);
#2262=EDGE_CURVE('',#1892,#1893,#1174,.T.);
#2263=EDGE_CURVE('',#1893,#1890,#1175,.T.);
#2264=EDGE_CURVE('',#1892,#1894,#1176,.T.);
#2265=EDGE_CURVE('',#1894,#1895,#1177,.T.);
#2266=EDGE_CURVE('',#1895,#1893,#1178,.T.);
#2267=EDGE_CURVE('',#1894,#1896,#1179,.T.);
#2268=EDGE_CURVE('',#1896,#1897,#1180,.T.);
#2269=EDGE_CURVE('',#1897,#1895,#1181,.T.);
#2270=EDGE_CURVE('',#1896,#1898,#1182,.T.);
#2271=EDGE_CURVE('',#1898,#1899,#1183,.T.);
#2272=EDGE_CURVE('',#1899,#1897,#1184,.T.);
#2273=EDGE_CURVE('',#1898,#1888,#1185,.T.);
#2274=EDGE_CURVE('',#1891,#1899,#1186,.T.);
#2275=EDGE_CURVE('',#1900,#1900,#1662,.T.);
#2276=EDGE_CURVE('',#1901,#1901,#1663,.T.);
#2277=EDGE_CURVE('',#1902,#1902,#1664,.T.);
#2278=EDGE_CURVE('',#1902,#1901,#1187,.T.);
#2279=EDGE_CURVE('',#1903,#1903,#1665,.T.);
#2280=EDGE_CURVE('',#1903,#1902,#1188,.T.);
#2281=EDGE_CURVE('',#1904,#1904,#1666,.T.);
#2282=EDGE_CURVE('',#1904,#1903,#1189,.T.);
#2283=EDGE_CURVE('',#1905,#1905,#1667,.T.);
#2284=EDGE_CURVE('',#1906,#1906,#1668,.F.);
#2285=EDGE_CURVE('',#1906,#1905,#1190,.T.);
#2286=EDGE_CURVE('',#1900,#1906,#1191,.T.);
#2287=EDGE_CURVE('',#1907,#1908,#1192,.T.);
#2288=EDGE_CURVE('',#1908,#1909,#1193,.T.);
#2289=EDGE_CURVE('',#1909,#1910,#1194,.T.);
#2290=EDGE_CURVE('',#1907,#1910,#1195,.T.);
#2291=EDGE_CURVE('',#1908,#1911,#1196,.T.);
#2292=EDGE_CURVE('',#1911,#1912,#1197,.T.);
#2293=EDGE_CURVE('',#1912,#1909,#1198,.T.);
#2294=EDGE_CURVE('',#1911,#1913,#1199,.T.);
#2295=EDGE_CURVE('',#1913,#1914,#1200,.T.);
#2296=EDGE_CURVE('',#1914,#1912,#1201,.T.);
#2297=EDGE_CURVE('',#1913,#1915,#1202,.T.);
#2298=EDGE_CURVE('',#1915,#1916,#1203,.T.);
#2299=EDGE_CURVE('',#1916,#1914,#1204,.T.);
#2300=EDGE_CURVE('',#1915,#1917,#1205,.T.);
#2301=EDGE_CURVE('',#1917,#1918,#1206,.T.);
#2302=EDGE_CURVE('',#1918,#1916,#1207,.T.);
#2303=EDGE_CURVE('',#1917,#1907,#1208,.T.);
#2304=EDGE_CURVE('',#1910,#1918,#1209,.T.);
#2305=EDGE_CURVE('',#1919,#1919,#1669,.T.);
#2306=EDGE_CURVE('',#1920,#1920,#1670,.T.);
#2307=EDGE_CURVE('',#1921,#1921,#1671,.T.);
#2308=EDGE_CURVE('',#1921,#1920,#1210,.T.);
#2309=EDGE_CURVE('',#1922,#1922,#1672,.T.);
#2310=EDGE_CURVE('',#1922,#1921,#1211,.T.);
#2311=EDGE_CURVE('',#1923,#1923,#1673,.T.);
#2312=EDGE_CURVE('',#1923,#1922,#1212,.T.);
#2313=EDGE_CURVE('',#1924,#1924,#1674,.T.);
#2314=EDGE_CURVE('',#1925,#1925,#1675,.F.);
#2315=EDGE_CURVE('',#1925,#1924,#1213,.T.);
#2316=EDGE_CURVE('',#1919,#1925,#1214,.T.);
#2317=EDGE_CURVE('',#1926,#1926,#1676,.T.);
#2318=EDGE_CURVE('',#1926,#1927,#1215,.T.);
#2319=EDGE_CURVE('',#1927,#1927,#1677,.T.);
#2320=EDGE_CURVE('',#1928,#1928,#1678,.T.);
#2321=EDGE_CURVE('',#1928,#1929,#1216,.T.);
#2322=EDGE_CURVE('',#1929,#1929,#1679,.T.);
#2323=EDGE_CURVE('',#1930,#1930,#1680,.T.);
#2324=EDGE_CURVE('',#1930,#1931,#1217,.T.);
#2325=EDGE_CURVE('',#1931,#1931,#1681,.T.);
#2326=EDGE_CURVE('',#1932,#1932,#1682,.T.);
#2327=EDGE_CURVE('',#1932,#1933,#1218,.T.);
#2328=EDGE_CURVE('',#1933,#1933,#1683,.T.);
#2329=EDGE_CURVE('',#1934,#1935,#1684,.T.);
#2330=EDGE_CURVE('',#1936,#1934,#1219,.T.);
#2331=EDGE_CURVE('',#1937,#1936,#1220,.T.);
#2332=EDGE_CURVE('',#1935,#1937,#1221,.T.);
#2333=EDGE_CURVE('',#1938,#1938,#1685,.T.);
#2334=EDGE_CURVE('',#1936,#1939,#1222,.T.);
#2335=EDGE_CURVE('',#1934,#1940,#1223,.T.);
#2336=EDGE_CURVE('',#1939,#1940,#1224,.T.);
#2337=EDGE_CURVE('',#1940,#1941,#1686,.T.);
#2338=EDGE_CURVE('',#1941,#1942,#1225,.T.);
#2339=EDGE_CURVE('',#1939,#1942,#1226,.T.);
#2340=EDGE_CURVE('',#1943,#1943,#1687,.T.);
#2341=EDGE_CURVE('',#1943,#1938,#1227,.T.);
#2342=EDGE_CURVE('',#1935,#1941,#1228,.T.);
#2343=EDGE_CURVE('',#1942,#1944,#1229,.T.);
#2344=EDGE_CURVE('',#1944,#1945,#1230,.T.);
#2345=EDGE_CURVE('',#1946,#1945,#1231,.T.);
#2346=EDGE_CURVE('',#1946,#1947,#1232,.T.);
#2347=EDGE_CURVE('',#1947,#1937,#1233,.T.);
#2348=EDGE_CURVE('',#1948,#1944,#1234,.T.);
#2349=EDGE_CURVE('',#1948,#1949,#1235,.T.);
#2350=EDGE_CURVE('',#1945,#1949,#1236,.T.);
#2351=EDGE_CURVE('',#1950,#1948,#1237,.T.);
#2352=EDGE_CURVE('',#1950,#1951,#1238,.T.);
#2353=EDGE_CURVE('',#1949,#1951,#1239,.T.);
#2354=EDGE_CURVE('',#1952,#1950,#1240,.T.);
#2355=EDGE_CURVE('',#1953,#1952,#1241,.T.);
#2356=EDGE_CURVE('',#1951,#1953,#1242,.T.);
#2357=EDGE_CURVE('',#1947,#1954,#1243,.T.);
#2358=EDGE_CURVE('',#1954,#1955,#1244,.T.);
#2359=EDGE_CURVE('',#1955,#1956,#1245,.T.);
#2360=EDGE_CURVE('',#1957,#1956,#1246,.T.);
#2361=EDGE_CURVE('',#1958,#1957,#1247,.T.);
#2362=EDGE_CURVE('',#1959,#1958,#1248,.T.);
#2363=EDGE_CURVE('',#1960,#1959,#1249,.T.);
#2364=EDGE_CURVE('',#1952,#1960,#1250,.T.);
#2365=EDGE_CURVE('',#1961,#1946,#1251,.T.);
#2366=EDGE_CURVE('',#1954,#1961,#1252,.T.);
#2367=EDGE_CURVE('',#1962,#1961,#1253,.T.);
#2368=EDGE_CURVE('',#1955,#1962,#1254,.T.);
#2369=EDGE_CURVE('',#1963,#1962,#1255,.T.);
#2370=EDGE_CURVE('',#1956,#1963,#1256,.T.);
#2371=EDGE_CURVE('',#1964,#1963,#1257,.T.);
#2372=EDGE_CURVE('',#1957,#1964,#1258,.T.);
#2373=EDGE_CURVE('',#1960,#1965,#1259,.T.);
#2374=EDGE_CURVE('',#1953,#1965,#1260,.T.);
#2375=EDGE_CURVE('',#1958,#1966,#1261,.T.);
#2376=EDGE_CURVE('',#1967,#1966,#1262,.T.);
#2377=EDGE_CURVE('',#1959,#1967,#1263,.T.);
#2378=EDGE_CURVE('',#1965,#1967,#1264,.T.);
#2379=EDGE_CURVE('',#1966,#1964,#1265,.T.);
#2380=EDGE_CURVE('',#1968,#1968,#1688,.T.);
#2381=EDGE_CURVE('',#1969,#1969,#1689,.T.);
#2382=EDGE_CURVE('',#1970,#1970,#1690,.T.);
#2383=EDGE_CURVE('',#1970,#1968,#1266,.T.);
#2384=EDGE_CURVE('',#1971,#1971,#1691,.T.);
#2385=EDGE_CURVE('',#1971,#1972,#1267,.T.);
#2386=EDGE_CURVE('',#1972,#1972,#1692,.T.);
#2387=EDGE_CURVE('',#1969,#1973,#1268,.T.);
#2388=EDGE_CURVE('',#1973,#1973,#1693,.T.);
#2389=EDGE_CURVE('',#1974,#1974,#1694,.T.);
#2390=EDGE_CURVE('',#1975,#1975,#1695,.T.);
#2391=EDGE_CURVE('',#1976,#1976,#1696,.T.);
#2392=EDGE_CURVE('',#1976,#1974,#1269,.T.);
#2393=EDGE_CURVE('',#1977,#1977,#1697,.T.);
#2394=EDGE_CURVE('',#1977,#1978,#1270,.T.);
#2395=EDGE_CURVE('',#1978,#1978,#1698,.T.);
#2396=EDGE_CURVE('',#1975,#1979,#1271,.T.);
#2397=EDGE_CURVE('',#1979,#1979,#1699,.T.);
#2398=EDGE_CURVE('',#1980,#1980,#1700,.T.);
#2399=EDGE_CURVE('',#1981,#1981,#1701,.T.);
#2400=EDGE_CURVE('',#1982,#1982,#1702,.T.);
#2401=EDGE_CURVE('',#1982,#1980,#1272,.T.);
#2402=EDGE_CURVE('',#1983,#1983,#1703,.T.);
#2403=EDGE_CURVE('',#1983,#1984,#1273,.T.);
#2404=EDGE_CURVE('',#1984,#1984,#1704,.T.);
#2405=EDGE_CURVE('',#1981,#1985,#1274,.T.);
#2406=EDGE_CURVE('',#1985,#1985,#1705,.T.);
#2407=EDGE_CURVE('',#1986,#1986,#1706,.T.);
#2408=EDGE_CURVE('',#1987,#1987,#1707,.T.);
#2409=EDGE_CURVE('',#1988,#1988,#1708,.T.);
#2410=EDGE_CURVE('',#1988,#1986,#1275,.T.);
#2411=EDGE_CURVE('',#1989,#1989,#1709,.T.);
#2412=EDGE_CURVE('',#1989,#1990,#1276,.T.);
#2413=EDGE_CURVE('',#1990,#1990,#1710,.T.);
#2414=EDGE_CURVE('',#1987,#1991,#1277,.T.);
#2415=EDGE_CURVE('',#1991,#1991,#1711,.T.);
#2416=EDGE_CURVE('',#1992,#1992,#1712,.T.);
#2417=EDGE_CURVE('',#1992,#1993,#1278,.T.);
#2418=EDGE_CURVE('',#1993,#1993,#1713,.T.);
#2419=EDGE_CURVE('',#1994,#1995,#1279,.T.);
#2420=EDGE_CURVE('',#1994,#1996,#1280,.T.);
#2421=EDGE_CURVE('',#1996,#1997,#1281,.T.);
#2422=EDGE_CURVE('',#1995,#1997,#1282,.T.);
#2423=EDGE_CURVE('',#1996,#1998,#1283,.T.);
#2424=EDGE_CURVE('',#1998,#1999,#1284,.T.);
#2425=EDGE_CURVE('',#1997,#1999,#1285,.T.);
#2426=EDGE_CURVE('',#2000,#2001,#1286,.T.);
#2427=EDGE_CURVE('',#1999,#2000,#1287,.T.);
#2428=EDGE_CURVE('',#1998,#2001,#1288,.T.);
#2429=EDGE_CURVE('',#2000,#1995,#1714,.T.);
#2430=EDGE_CURVE('',#2001,#1994,#1715,.T.);
#2431=EDGE_CURVE('',#2002,#2002,#1716,.T.);
#2432=EDGE_CURVE('',#2002,#2003,#1289,.T.);
#2433=EDGE_CURVE('',#2003,#2003,#1717,.T.);
#2434=EDGE_CURVE('',#2004,#2004,#1718,.T.);
#2435=EDGE_CURVE('',#2004,#2005,#1290,.T.);
#2436=EDGE_CURVE('',#2005,#2005,#1719,.T.);
#2437=ORIENTED_EDGE('',*,*,#2006,.F.);
#2438=ORIENTED_EDGE('',*,*,#2007,.T.);
#2439=ORIENTED_EDGE('',*,*,#2008,.F.);
#2440=ORIENTED_EDGE('',*,*,#2007,.F.);
#2441=ORIENTED_EDGE('',*,*,#2009,.F.);
#2442=ORIENTED_EDGE('',*,*,#2010,.T.);
#2443=ORIENTED_EDGE('',*,*,#2011,.F.);
#2444=ORIENTED_EDGE('',*,*,#2010,.F.);
#2445=ORIENTED_EDGE('',*,*,#2012,.F.);
#2446=ORIENTED_EDGE('',*,*,#2013,.T.);
#2447=ORIENTED_EDGE('',*,*,#2014,.F.);
#2448=ORIENTED_EDGE('',*,*,#2013,.F.);
#2449=ORIENTED_EDGE('',*,*,#2015,.F.);
#2450=ORIENTED_EDGE('',*,*,#2016,.T.);
#2451=ORIENTED_EDGE('',*,*,#2017,.F.);
#2452=ORIENTED_EDGE('',*,*,#2016,.F.);
#2453=ORIENTED_EDGE('',*,*,#2018,.F.);
#2454=ORIENTED_EDGE('',*,*,#2019,.T.);
#2455=ORIENTED_EDGE('',*,*,#2020,.F.);
#2456=ORIENTED_EDGE('',*,*,#2019,.F.);
#2457=ORIENTED_EDGE('',*,*,#2021,.F.);
#2458=ORIENTED_EDGE('',*,*,#2022,.T.);
#2459=ORIENTED_EDGE('',*,*,#2023,.F.);
#2460=ORIENTED_EDGE('',*,*,#2022,.F.);
#2461=ORIENTED_EDGE('',*,*,#2024,.F.);
#2462=ORIENTED_EDGE('',*,*,#2025,.T.);
#2463=ORIENTED_EDGE('',*,*,#2026,.F.);
#2464=ORIENTED_EDGE('',*,*,#2025,.F.);
#2465=ORIENTED_EDGE('',*,*,#2027,.F.);
#2466=ORIENTED_EDGE('',*,*,#2028,.T.);
#2467=ORIENTED_EDGE('',*,*,#2029,.F.);
#2468=ORIENTED_EDGE('',*,*,#2028,.F.);
#2469=ORIENTED_EDGE('',*,*,#2030,.F.);
#2470=ORIENTED_EDGE('',*,*,#2031,.T.);
#2471=ORIENTED_EDGE('',*,*,#2032,.F.);
#2472=ORIENTED_EDGE('',*,*,#2031,.F.);
#2473=ORIENTED_EDGE('',*,*,#2033,.F.);
#2474=ORIENTED_EDGE('',*,*,#2034,.T.);
#2475=ORIENTED_EDGE('',*,*,#2035,.F.);
#2476=ORIENTED_EDGE('',*,*,#2034,.F.);
#2477=ORIENTED_EDGE('',*,*,#2036,.F.);
#2478=ORIENTED_EDGE('',*,*,#2037,.T.);
#2479=ORIENTED_EDGE('',*,*,#2038,.F.);
#2480=ORIENTED_EDGE('',*,*,#2037,.F.);
#2481=ORIENTED_EDGE('',*,*,#2039,.F.);
#2482=ORIENTED_EDGE('',*,*,#2040,.T.);
#2483=ORIENTED_EDGE('',*,*,#2041,.F.);
#2484=ORIENTED_EDGE('',*,*,#2040,.F.);
#2485=ORIENTED_EDGE('',*,*,#2042,.F.);
#2486=ORIENTED_EDGE('',*,*,#2043,.T.);
#2487=ORIENTED_EDGE('',*,*,#2044,.F.);
#2488=ORIENTED_EDGE('',*,*,#2043,.F.);
#2489=ORIENTED_EDGE('',*,*,#2045,.F.);
#2490=ORIENTED_EDGE('',*,*,#2046,.T.);
#2491=ORIENTED_EDGE('',*,*,#2047,.F.);
#2492=ORIENTED_EDGE('',*,*,#2046,.F.);
#2493=ORIENTED_EDGE('',*,*,#2048,.T.);
#2494=ORIENTED_EDGE('',*,*,#2049,.T.);
#2495=ORIENTED_EDGE('',*,*,#2050,.F.);
#2496=ORIENTED_EDGE('',*,*,#2051,.F.);
#2497=ORIENTED_EDGE('',*,*,#2052,.T.);
#2498=ORIENTED_EDGE('',*,*,#2051,.T.);
#2499=ORIENTED_EDGE('',*,*,#2053,.F.);
#2500=ORIENTED_EDGE('',*,*,#2054,.F.);
#2501=ORIENTED_EDGE('',*,*,#2055,.T.);
#2502=ORIENTED_EDGE('',*,*,#2054,.T.);
#2503=ORIENTED_EDGE('',*,*,#2056,.F.);
#2504=ORIENTED_EDGE('',*,*,#2057,.F.);
#2505=ORIENTED_EDGE('',*,*,#2058,.T.);
#2506=ORIENTED_EDGE('',*,*,#2057,.T.);
#2507=ORIENTED_EDGE('',*,*,#2059,.F.);
#2508=ORIENTED_EDGE('',*,*,#2049,.F.);
#2509=ORIENTED_EDGE('',*,*,#2059,.T.);
#2510=ORIENTED_EDGE('',*,*,#2056,.T.);
#2511=ORIENTED_EDGE('',*,*,#2053,.T.);
#2512=ORIENTED_EDGE('',*,*,#2050,.T.);
#2513=ORIENTED_EDGE('',*,*,#2014,.T.);
#2514=ORIENTED_EDGE('',*,*,#2017,.T.);
#2515=ORIENTED_EDGE('',*,*,#2020,.T.);
#2516=ORIENTED_EDGE('',*,*,#2023,.T.);
#2517=ORIENTED_EDGE('',*,*,#2047,.T.);
#2518=ORIENTED_EDGE('',*,*,#2044,.T.);
#2519=ORIENTED_EDGE('',*,*,#2041,.T.);
#2520=ORIENTED_EDGE('',*,*,#2038,.T.);
#2521=ORIENTED_EDGE('',*,*,#2035,.T.);
#2522=ORIENTED_EDGE('',*,*,#2032,.T.);
#2523=ORIENTED_EDGE('',*,*,#2029,.T.);
#2524=ORIENTED_EDGE('',*,*,#2026,.T.);
#2525=ORIENTED_EDGE('',*,*,#2011,.T.);
#2526=ORIENTED_EDGE('',*,*,#2008,.T.);
#2527=ORIENTED_EDGE('',*,*,#2058,.F.);
#2528=ORIENTED_EDGE('',*,*,#2048,.F.);
#2529=ORIENTED_EDGE('',*,*,#2052,.F.);
#2530=ORIENTED_EDGE('',*,*,#2055,.F.);
#2531=ORIENTED_EDGE('',*,*,#2012,.T.);
#2532=ORIENTED_EDGE('',*,*,#2015,.T.);
#2533=ORIENTED_EDGE('',*,*,#2018,.T.);
#2534=ORIENTED_EDGE('',*,*,#2021,.T.);
#2535=ORIENTED_EDGE('',*,*,#2045,.T.);
#2536=ORIENTED_EDGE('',*,*,#2042,.T.);
#2537=ORIENTED_EDGE('',*,*,#2039,.T.);
#2538=ORIENTED_EDGE('',*,*,#2036,.T.);
#2539=ORIENTED_EDGE('',*,*,#2033,.T.);
#2540=ORIENTED_EDGE('',*,*,#2030,.T.);
#2541=ORIENTED_EDGE('',*,*,#2027,.T.);
#2542=ORIENTED_EDGE('',*,*,#2024,.T.);
#2543=ORIENTED_EDGE('',*,*,#2009,.T.);
#2544=ORIENTED_EDGE('',*,*,#2006,.T.);
#2545=ORIENTED_EDGE('',*,*,#2060,.F.);
#2546=ORIENTED_EDGE('',*,*,#2061,.T.);
#2547=ORIENTED_EDGE('',*,*,#2062,.T.);
#2548=ORIENTED_EDGE('',*,*,#2061,.F.);
#2549=ORIENTED_EDGE('',*,*,#2060,.T.);
#2550=ORIENTED_EDGE('',*,*,#2062,.F.);
#2551=ORIENTED_EDGE('',*,*,#2063,.F.);
#2552=ORIENTED_EDGE('',*,*,#2064,.T.);
#2553=ORIENTED_EDGE('',*,*,#2065,.T.);
#2554=ORIENTED_EDGE('',*,*,#2064,.F.);
#2555=ORIENTED_EDGE('',*,*,#2063,.T.);
#2556=ORIENTED_EDGE('',*,*,#2065,.F.);
#2557=ORIENTED_EDGE('',*,*,#2066,.F.);
#2558=ORIENTED_EDGE('',*,*,#2067,.T.);
#2559=ORIENTED_EDGE('',*,*,#2068,.T.);
#2560=ORIENTED_EDGE('',*,*,#2067,.F.);
#2561=ORIENTED_EDGE('',*,*,#2066,.T.);
#2562=ORIENTED_EDGE('',*,*,#2068,.F.);
#2563=ORIENTED_EDGE('',*,*,#2069,.F.);
#2564=ORIENTED_EDGE('',*,*,#2070,.T.);
#2565=ORIENTED_EDGE('',*,*,#2071,.T.);
#2566=ORIENTED_EDGE('',*,*,#2070,.F.);
#2567=ORIENTED_EDGE('',*,*,#2069,.T.);
#2568=ORIENTED_EDGE('',*,*,#2071,.F.);
#2569=ORIENTED_EDGE('',*,*,#2072,.F.);
#2570=ORIENTED_EDGE('',*,*,#2073,.T.);
#2571=ORIENTED_EDGE('',*,*,#2074,.F.);
#2572=ORIENTED_EDGE('',*,*,#2073,.F.);
#2573=ORIENTED_EDGE('',*,*,#2072,.T.);
#2574=ORIENTED_EDGE('',*,*,#2075,.F.);
#2575=ORIENTED_EDGE('',*,*,#2076,.F.);
#2576=ORIENTED_EDGE('',*,*,#2077,.T.);
#2577=ORIENTED_EDGE('',*,*,#2078,.F.);
#2578=ORIENTED_EDGE('',*,*,#2077,.F.);
#2579=ORIENTED_EDGE('',*,*,#2076,.T.);
#2580=ORIENTED_EDGE('',*,*,#2079,.F.);
#2581=ORIENTED_EDGE('',*,*,#2080,.F.);
#2582=ORIENTED_EDGE('',*,*,#2081,.T.);
#2583=ORIENTED_EDGE('',*,*,#2082,.F.);
#2584=ORIENTED_EDGE('',*,*,#2081,.F.);
#2585=ORIENTED_EDGE('',*,*,#2080,.T.);
#2586=ORIENTED_EDGE('',*,*,#2083,.F.);
#2587=ORIENTED_EDGE('',*,*,#2084,.F.);
#2588=ORIENTED_EDGE('',*,*,#2085,.T.);
#2589=ORIENTED_EDGE('',*,*,#2086,.F.);
#2590=ORIENTED_EDGE('',*,*,#2085,.F.);
#2591=ORIENTED_EDGE('',*,*,#2084,.T.);
#2592=ORIENTED_EDGE('',*,*,#2087,.F.);
#2593=ORIENTED_EDGE('',*,*,#2088,.F.);
#2594=ORIENTED_EDGE('',*,*,#2089,.T.);
#2595=ORIENTED_EDGE('',*,*,#2075,.T.);
#2596=ORIENTED_EDGE('',*,*,#2089,.F.);
#2597=ORIENTED_EDGE('',*,*,#2090,.F.);
#2598=ORIENTED_EDGE('',*,*,#2091,.T.);
#2599=ORIENTED_EDGE('',*,*,#2079,.T.);
#2600=ORIENTED_EDGE('',*,*,#2091,.F.);
#2601=ORIENTED_EDGE('',*,*,#2092,.F.);
#2602=ORIENTED_EDGE('',*,*,#2093,.T.);
#2603=ORIENTED_EDGE('',*,*,#2083,.T.);
#2604=ORIENTED_EDGE('',*,*,#2093,.F.);
#2605=ORIENTED_EDGE('',*,*,#2094,.F.);
#2606=ORIENTED_EDGE('',*,*,#2095,.T.);
#2607=ORIENTED_EDGE('',*,*,#2087,.T.);
#2608=ORIENTED_EDGE('',*,*,#2095,.F.);
#2609=ORIENTED_EDGE('',*,*,#2096,.F.);
#2610=ORIENTED_EDGE('',*,*,#2097,.F.);
#2611=ORIENTED_EDGE('',*,*,#2098,.F.);
#2612=ORIENTED_EDGE('',*,*,#2099,.T.);
#2613=ORIENTED_EDGE('',*,*,#2100,.F.);
#2614=ORIENTED_EDGE('',*,*,#2099,.F.);
#2615=ORIENTED_EDGE('',*,*,#2101,.F.);
#2616=ORIENTED_EDGE('',*,*,#2102,.T.);
#2617=ORIENTED_EDGE('',*,*,#2103,.F.);
#2618=ORIENTED_EDGE('',*,*,#2102,.F.);
#2619=ORIENTED_EDGE('',*,*,#2104,.F.);
#2620=ORIENTED_EDGE('',*,*,#2105,.T.);
#2621=ORIENTED_EDGE('',*,*,#2106,.F.);
#2622=ORIENTED_EDGE('',*,*,#2105,.F.);
#2623=ORIENTED_EDGE('',*,*,#2107,.F.);
#2624=ORIENTED_EDGE('',*,*,#2097,.T.);
#2625=ORIENTED_EDGE('',*,*,#2101,.T.);
#2626=ORIENTED_EDGE('',*,*,#2098,.T.);
#2627=ORIENTED_EDGE('',*,*,#2107,.T.);
#2628=ORIENTED_EDGE('',*,*,#2104,.T.);
#2629=ORIENTED_EDGE('',*,*,#2108,.T.);
#2630=ORIENTED_EDGE('',*,*,#2109,.T.);
#2631=ORIENTED_EDGE('',*,*,#2110,.F.);
#2632=ORIENTED_EDGE('',*,*,#2111,.F.);
#2633=ORIENTED_EDGE('',*,*,#2112,.T.);
#2634=ORIENTED_EDGE('',*,*,#2111,.T.);
#2635=ORIENTED_EDGE('',*,*,#2113,.F.);
#2636=ORIENTED_EDGE('',*,*,#2114,.F.);
#2637=ORIENTED_EDGE('',*,*,#2115,.T.);
#2638=ORIENTED_EDGE('',*,*,#2114,.T.);
#2639=ORIENTED_EDGE('',*,*,#2116,.F.);
#2640=ORIENTED_EDGE('',*,*,#2117,.F.);
#2641=ORIENTED_EDGE('',*,*,#2118,.T.);
#2642=ORIENTED_EDGE('',*,*,#2117,.T.);
#2643=ORIENTED_EDGE('',*,*,#2119,.F.);
#2644=ORIENTED_EDGE('',*,*,#2109,.F.);
#2645=ORIENTED_EDGE('',*,*,#2119,.T.);
#2646=ORIENTED_EDGE('',*,*,#2116,.T.);
#2647=ORIENTED_EDGE('',*,*,#2113,.T.);
#2648=ORIENTED_EDGE('',*,*,#2110,.T.);
#2649=ORIENTED_EDGE('',*,*,#2103,.T.);
#2650=ORIENTED_EDGE('',*,*,#2106,.T.);
#2651=ORIENTED_EDGE('',*,*,#2096,.T.);
#2652=ORIENTED_EDGE('',*,*,#2100,.T.);
#2653=ORIENTED_EDGE('',*,*,#2086,.T.);
#2654=ORIENTED_EDGE('',*,*,#2082,.T.);
#2655=ORIENTED_EDGE('',*,*,#2078,.T.);
#2656=ORIENTED_EDGE('',*,*,#2074,.T.);
#2657=ORIENTED_EDGE('',*,*,#2118,.F.);
#2658=ORIENTED_EDGE('',*,*,#2108,.F.);
#2659=ORIENTED_EDGE('',*,*,#2112,.F.);
#2660=ORIENTED_EDGE('',*,*,#2115,.F.);
#2661=ORIENTED_EDGE('',*,*,#2088,.T.);
#2662=ORIENTED_EDGE('',*,*,#2090,.T.);
#2663=ORIENTED_EDGE('',*,*,#2092,.T.);
#2664=ORIENTED_EDGE('',*,*,#2094,.T.);
#2665=ORIENTED_EDGE('',*,*,#2120,.T.);
#2666=ORIENTED_EDGE('',*,*,#2121,.T.);
#2667=ORIENTED_EDGE('',*,*,#2122,.F.);
#2668=ORIENTED_EDGE('',*,*,#2123,.F.);
#2669=ORIENTED_EDGE('',*,*,#2124,.T.);
#2670=ORIENTED_EDGE('',*,*,#2123,.T.);
#2671=ORIENTED_EDGE('',*,*,#2125,.F.);
#2672=ORIENTED_EDGE('',*,*,#2126,.F.);
#2673=ORIENTED_EDGE('',*,*,#2127,.T.);
#2674=ORIENTED_EDGE('',*,*,#2126,.T.);
#2675=ORIENTED_EDGE('',*,*,#2128,.F.);
#2676=ORIENTED_EDGE('',*,*,#2129,.F.);
#2677=ORIENTED_EDGE('',*,*,#2130,.T.);
#2678=ORIENTED_EDGE('',*,*,#2129,.T.);
#2679=ORIENTED_EDGE('',*,*,#2131,.F.);
#2680=ORIENTED_EDGE('',*,*,#2121,.F.);
#2681=ORIENTED_EDGE('',*,*,#2131,.T.);
#2682=ORIENTED_EDGE('',*,*,#2128,.T.);
#2683=ORIENTED_EDGE('',*,*,#2125,.T.);
#2684=ORIENTED_EDGE('',*,*,#2122,.T.);
#2685=ORIENTED_EDGE('',*,*,#2130,.F.);
#2686=ORIENTED_EDGE('',*,*,#2120,.F.);
#2687=ORIENTED_EDGE('',*,*,#2124,.F.);
#2688=ORIENTED_EDGE('',*,*,#2127,.F.);
#2689=ORIENTED_EDGE('',*,*,#2132,.F.);
#2690=ORIENTED_EDGE('',*,*,#2133,.T.);
#2691=ORIENTED_EDGE('',*,*,#2134,.F.);
#2692=ORIENTED_EDGE('',*,*,#2133,.F.);
#2693=ORIENTED_EDGE('',*,*,#2135,.F.);
#2694=ORIENTED_EDGE('',*,*,#2132,.T.);
#2695=ORIENTED_EDGE('',*,*,#2136,.F.);
#2696=ORIENTED_EDGE('',*,*,#2137,.F.);
#2697=ORIENTED_EDGE('',*,*,#2138,.T.);
#2698=ORIENTED_EDGE('',*,*,#2136,.T.);
#2699=ORIENTED_EDGE('',*,*,#2138,.F.);
#2700=ORIENTED_EDGE('',*,*,#2139,.F.);
#2701=ORIENTED_EDGE('',*,*,#2140,.T.);
#2702=ORIENTED_EDGE('',*,*,#2141,.F.);
#2703=ORIENTED_EDGE('',*,*,#2140,.F.);
#2704=ORIENTED_EDGE('',*,*,#2142,.F.);
#2705=ORIENTED_EDGE('',*,*,#2143,.T.);
#2706=ORIENTED_EDGE('',*,*,#2144,.F.);
#2707=ORIENTED_EDGE('',*,*,#2143,.F.);
#2708=ORIENTED_EDGE('',*,*,#2135,.T.);
#2709=ORIENTED_EDGE('',*,*,#2145,.T.);
#2710=ORIENTED_EDGE('',*,*,#2146,.T.);
#2711=ORIENTED_EDGE('',*,*,#2147,.F.);
#2712=ORIENTED_EDGE('',*,*,#2148,.F.);
#2713=ORIENTED_EDGE('',*,*,#2134,.T.);
#2714=ORIENTED_EDGE('',*,*,#2149,.T.);
#2715=ORIENTED_EDGE('',*,*,#2148,.T.);
#2716=ORIENTED_EDGE('',*,*,#2150,.F.);
#2717=ORIENTED_EDGE('',*,*,#2151,.F.);
#2718=ORIENTED_EDGE('',*,*,#2152,.T.);
#2719=ORIENTED_EDGE('',*,*,#2151,.T.);
#2720=ORIENTED_EDGE('',*,*,#2153,.F.);
#2721=ORIENTED_EDGE('',*,*,#2154,.F.);
#2722=ORIENTED_EDGE('',*,*,#2141,.T.);
#2723=ORIENTED_EDGE('',*,*,#2155,.T.);
#2724=ORIENTED_EDGE('',*,*,#2154,.T.);
#2725=ORIENTED_EDGE('',*,*,#2156,.F.);
#2726=ORIENTED_EDGE('',*,*,#2157,.F.);
#2727=ORIENTED_EDGE('',*,*,#2158,.T.);
#2728=ORIENTED_EDGE('',*,*,#2157,.T.);
#2729=ORIENTED_EDGE('',*,*,#2159,.F.);
#2730=ORIENTED_EDGE('',*,*,#2160,.F.);
#2731=ORIENTED_EDGE('',*,*,#2137,.T.);
#2732=ORIENTED_EDGE('',*,*,#2139,.T.);
#2733=ORIENTED_EDGE('',*,*,#2161,.T.);
#2734=ORIENTED_EDGE('',*,*,#2160,.T.);
#2735=ORIENTED_EDGE('',*,*,#2162,.F.);
#2736=ORIENTED_EDGE('',*,*,#2146,.F.);
#2737=ORIENTED_EDGE('',*,*,#2162,.T.);
#2738=ORIENTED_EDGE('',*,*,#2159,.T.);
#2739=ORIENTED_EDGE('',*,*,#2156,.T.);
#2740=ORIENTED_EDGE('',*,*,#2153,.T.);
#2741=ORIENTED_EDGE('',*,*,#2150,.T.);
#2742=ORIENTED_EDGE('',*,*,#2147,.T.);
#2743=ORIENTED_EDGE('',*,*,#2144,.T.);
#2744=ORIENTED_EDGE('',*,*,#2161,.F.);
#2745=ORIENTED_EDGE('',*,*,#2145,.F.);
#2746=ORIENTED_EDGE('',*,*,#2149,.F.);
#2747=ORIENTED_EDGE('',*,*,#2152,.F.);
#2748=ORIENTED_EDGE('',*,*,#2155,.F.);
#2749=ORIENTED_EDGE('',*,*,#2158,.F.);
#2750=ORIENTED_EDGE('',*,*,#2142,.T.);
#2751=ORIENTED_EDGE('',*,*,#2163,.F.);
#2752=ORIENTED_EDGE('',*,*,#2164,.T.);
#2753=ORIENTED_EDGE('',*,*,#2165,.F.);
#2754=ORIENTED_EDGE('',*,*,#2164,.F.);
#2755=ORIENTED_EDGE('',*,*,#2166,.F.);
#2756=ORIENTED_EDGE('',*,*,#2163,.T.);
#2757=ORIENTED_EDGE('',*,*,#2167,.F.);
#2758=ORIENTED_EDGE('',*,*,#2168,.F.);
#2759=ORIENTED_EDGE('',*,*,#2169,.T.);
#2760=ORIENTED_EDGE('',*,*,#2167,.T.);
#2761=ORIENTED_EDGE('',*,*,#2169,.F.);
#2762=ORIENTED_EDGE('',*,*,#2170,.F.);
#2763=ORIENTED_EDGE('',*,*,#2171,.T.);
#2764=ORIENTED_EDGE('',*,*,#2172,.F.);
#2765=ORIENTED_EDGE('',*,*,#2171,.F.);
#2766=ORIENTED_EDGE('',*,*,#2173,.F.);
#2767=ORIENTED_EDGE('',*,*,#2174,.T.);
#2768=ORIENTED_EDGE('',*,*,#2175,.F.);
#2769=ORIENTED_EDGE('',*,*,#2174,.F.);
#2770=ORIENTED_EDGE('',*,*,#2166,.T.);
#2771=ORIENTED_EDGE('',*,*,#2176,.T.);
#2772=ORIENTED_EDGE('',*,*,#2177,.T.);
#2773=ORIENTED_EDGE('',*,*,#2178,.F.);
#2774=ORIENTED_EDGE('',*,*,#2179,.F.);
#2775=ORIENTED_EDGE('',*,*,#2165,.T.);
#2776=ORIENTED_EDGE('',*,*,#2180,.T.);
#2777=ORIENTED_EDGE('',*,*,#2179,.T.);
#2778=ORIENTED_EDGE('',*,*,#2181,.F.);
#2779=ORIENTED_EDGE('',*,*,#2182,.F.);
#2780=ORIENTED_EDGE('',*,*,#2183,.T.);
#2781=ORIENTED_EDGE('',*,*,#2182,.T.);
#2782=ORIENTED_EDGE('',*,*,#2184,.F.);
#2783=ORIENTED_EDGE('',*,*,#2185,.F.);
#2784=ORIENTED_EDGE('',*,*,#2172,.T.);
#2785=ORIENTED_EDGE('',*,*,#2186,.T.);
#2786=ORIENTED_EDGE('',*,*,#2185,.T.);
#2787=ORIENTED_EDGE('',*,*,#2187,.F.);
#2788=ORIENTED_EDGE('',*,*,#2188,.F.);
#2789=ORIENTED_EDGE('',*,*,#2189,.T.);
#2790=ORIENTED_EDGE('',*,*,#2188,.T.);
#2791=ORIENTED_EDGE('',*,*,#2190,.F.);
#2792=ORIENTED_EDGE('',*,*,#2191,.F.);
#2793=ORIENTED_EDGE('',*,*,#2168,.T.);
#2794=ORIENTED_EDGE('',*,*,#2170,.T.);
#2795=ORIENTED_EDGE('',*,*,#2192,.T.);
#2796=ORIENTED_EDGE('',*,*,#2191,.T.);
#2797=ORIENTED_EDGE('',*,*,#2193,.F.);
#2798=ORIENTED_EDGE('',*,*,#2177,.F.);
#2799=ORIENTED_EDGE('',*,*,#2193,.T.);
#2800=ORIENTED_EDGE('',*,*,#2190,.T.);
#2801=ORIENTED_EDGE('',*,*,#2187,.T.);
#2802=ORIENTED_EDGE('',*,*,#2184,.T.);
#2803=ORIENTED_EDGE('',*,*,#2181,.T.);
#2804=ORIENTED_EDGE('',*,*,#2178,.T.);
#2805=ORIENTED_EDGE('',*,*,#2175,.T.);
#2806=ORIENTED_EDGE('',*,*,#2192,.F.);
#2807=ORIENTED_EDGE('',*,*,#2176,.F.);
#2808=ORIENTED_EDGE('',*,*,#2180,.F.);
#2809=ORIENTED_EDGE('',*,*,#2183,.F.);
#2810=ORIENTED_EDGE('',*,*,#2186,.F.);
#2811=ORIENTED_EDGE('',*,*,#2189,.F.);
#2812=ORIENTED_EDGE('',*,*,#2173,.T.);
#2813=ORIENTED_EDGE('',*,*,#2194,.F.);
#2814=ORIENTED_EDGE('',*,*,#2195,.T.);
#2815=ORIENTED_EDGE('',*,*,#2196,.F.);
#2816=ORIENTED_EDGE('',*,*,#2195,.F.);
#2817=ORIENTED_EDGE('',*,*,#2194,.T.);
#2818=ORIENTED_EDGE('',*,*,#2197,.F.);
#2819=ORIENTED_EDGE('',*,*,#2198,.T.);
#2820=ORIENTED_EDGE('',*,*,#2199,.T.);
#2821=ORIENTED_EDGE('',*,*,#2198,.F.);
#2822=ORIENTED_EDGE('',*,*,#2199,.F.);
#2823=ORIENTED_EDGE('',*,*,#2200,.F.);
#2824=ORIENTED_EDGE('',*,*,#2201,.T.);
#2825=ORIENTED_EDGE('',*,*,#2202,.T.);
#2826=ORIENTED_EDGE('',*,*,#2201,.F.);
#2827=ORIENTED_EDGE('',*,*,#2200,.T.);
#2828=ORIENTED_EDGE('',*,*,#2196,.T.);
#2829=ORIENTED_EDGE('',*,*,#2202,.F.);
#2830=ORIENTED_EDGE('',*,*,#2197,.T.);
#2831=ORIENTED_EDGE('',*,*,#2203,.F.);
#2832=ORIENTED_EDGE('',*,*,#2204,.T.);
#2833=ORIENTED_EDGE('',*,*,#2205,.T.);
#2834=ORIENTED_EDGE('',*,*,#2204,.F.);
#2835=ORIENTED_EDGE('',*,*,#2206,.F.);
#2836=ORIENTED_EDGE('',*,*,#2207,.T.);
#2837=ORIENTED_EDGE('',*,*,#2208,.T.);
#2838=ORIENTED_EDGE('',*,*,#2207,.F.);
#2839=ORIENTED_EDGE('',*,*,#2206,.T.);
#2840=ORIENTED_EDGE('',*,*,#2203,.T.);
#2841=ORIENTED_EDGE('',*,*,#2208,.F.);
#2842=ORIENTED_EDGE('',*,*,#2205,.F.);
#2843=ORIENTED_EDGE('',*,*,#2209,.F.);
#2844=ORIENTED_EDGE('',*,*,#2210,.T.);
#2845=ORIENTED_EDGE('',*,*,#2211,.T.);
#2846=ORIENTED_EDGE('',*,*,#2210,.F.);
#2847=ORIENTED_EDGE('',*,*,#2212,.F.);
#2848=ORIENTED_EDGE('',*,*,#2213,.T.);
#2849=ORIENTED_EDGE('',*,*,#2214,.T.);
#2850=ORIENTED_EDGE('',*,*,#2213,.F.);
#2851=ORIENTED_EDGE('',*,*,#2212,.T.);
#2852=ORIENTED_EDGE('',*,*,#2209,.T.);
#2853=ORIENTED_EDGE('',*,*,#2214,.F.);
#2854=ORIENTED_EDGE('',*,*,#2211,.F.);
#2855=ORIENTED_EDGE('',*,*,#2215,.F.);
#2856=ORIENTED_EDGE('',*,*,#2216,.T.);
#2857=ORIENTED_EDGE('',*,*,#2217,.F.);
#2858=ORIENTED_EDGE('',*,*,#2216,.F.);
#2859=ORIENTED_EDGE('',*,*,#2215,.T.);
#2860=ORIENTED_EDGE('',*,*,#2218,.F.);
#2861=ORIENTED_EDGE('',*,*,#2219,.F.);
#2862=ORIENTED_EDGE('',*,*,#2220,.F.);
#2863=ORIENTED_EDGE('',*,*,#2221,.T.);
#2864=ORIENTED_EDGE('',*,*,#2222,.F.);
#2865=ORIENTED_EDGE('',*,*,#2223,.F.);
#2866=ORIENTED_EDGE('',*,*,#2219,.T.);
#2867=ORIENTED_EDGE('',*,*,#2224,.F.);
#2868=ORIENTED_EDGE('',*,*,#2225,.F.);
#2869=ORIENTED_EDGE('',*,*,#2221,.F.);
#2870=ORIENTED_EDGE('',*,*,#2226,.F.);
#2871=ORIENTED_EDGE('',*,*,#2227,.F.);
#2872=ORIENTED_EDGE('',*,*,#2228,.F.);
#2873=ORIENTED_EDGE('',*,*,#2229,.T.);
#2874=ORIENTED_EDGE('',*,*,#2230,.F.);
#2875=ORIENTED_EDGE('',*,*,#2231,.F.);
#2876=ORIENTED_EDGE('',*,*,#2227,.T.);
#2877=ORIENTED_EDGE('',*,*,#2232,.F.);
#2878=ORIENTED_EDGE('',*,*,#2233,.F.);
#2879=ORIENTED_EDGE('',*,*,#2229,.F.);
#2880=ORIENTED_EDGE('',*,*,#2234,.F.);
#2881=ORIENTED_EDGE('',*,*,#2235,.T.);
#2882=ORIENTED_EDGE('',*,*,#2236,.T.);
#2883=ORIENTED_EDGE('',*,*,#2224,.T.);
#2884=ORIENTED_EDGE('',*,*,#2218,.T.);
#2885=ORIENTED_EDGE('',*,*,#2223,.T.);
#2886=ORIENTED_EDGE('',*,*,#2237,.T.);
#2887=ORIENTED_EDGE('',*,*,#2232,.T.);
#2888=ORIENTED_EDGE('',*,*,#2226,.T.);
#2889=ORIENTED_EDGE('',*,*,#2231,.T.);
#2890=ORIENTED_EDGE('',*,*,#2238,.T.);
#2891=ORIENTED_EDGE('',*,*,#2235,.F.);
#2892=ORIENTED_EDGE('',*,*,#2239,.T.);
#2893=ORIENTED_EDGE('',*,*,#2222,.T.);
#2894=ORIENTED_EDGE('',*,*,#2225,.T.);
#2895=ORIENTED_EDGE('',*,*,#2236,.F.);
#2896=ORIENTED_EDGE('',*,*,#2238,.F.);
#2897=ORIENTED_EDGE('',*,*,#2230,.T.);
#2898=ORIENTED_EDGE('',*,*,#2233,.T.);
#2899=ORIENTED_EDGE('',*,*,#2237,.F.);
#2900=ORIENTED_EDGE('',*,*,#2239,.F.);
#2901=ORIENTED_EDGE('',*,*,#2240,.T.);
#2902=ORIENTED_EDGE('',*,*,#2241,.T.);
#2903=ORIENTED_EDGE('',*,*,#2240,.F.);
#2904=ORIENTED_EDGE('',*,*,#2242,.F.);
#2905=ORIENTED_EDGE('',*,*,#2243,.T.);
#2906=ORIENTED_EDGE('',*,*,#2244,.F.);
#2907=ORIENTED_EDGE('',*,*,#2243,.F.);
#2908=ORIENTED_EDGE('',*,*,#2242,.T.);
#2909=ORIENTED_EDGE('',*,*,#2217,.T.);
#2910=ORIENTED_EDGE('',*,*,#2234,.T.);
#2911=ORIENTED_EDGE('',*,*,#2244,.T.);
#2912=ORIENTED_EDGE('',*,*,#2241,.F.);
#2913=ORIENTED_EDGE('',*,*,#2220,.T.);
#2914=ORIENTED_EDGE('',*,*,#2228,.T.);
#2915=ORIENTED_EDGE('',*,*,#2245,.F.);
#2916=ORIENTED_EDGE('',*,*,#2246,.T.);
#2917=ORIENTED_EDGE('',*,*,#2247,.T.);
#2918=ORIENTED_EDGE('',*,*,#2246,.F.);
#2919=ORIENTED_EDGE('',*,*,#2248,.F.);
#2920=ORIENTED_EDGE('',*,*,#2249,.T.);
#2921=ORIENTED_EDGE('',*,*,#2250,.T.);
#2922=ORIENTED_EDGE('',*,*,#2249,.F.);
#2923=ORIENTED_EDGE('',*,*,#2248,.T.);
#2924=ORIENTED_EDGE('',*,*,#2245,.T.);
#2925=ORIENTED_EDGE('',*,*,#2250,.F.);
#2926=ORIENTED_EDGE('',*,*,#2247,.F.);
#2927=ORIENTED_EDGE('',*,*,#2251,.F.);
#2928=ORIENTED_EDGE('',*,*,#2252,.T.);
#2929=ORIENTED_EDGE('',*,*,#2253,.T.);
#2930=ORIENTED_EDGE('',*,*,#2252,.F.);
#2931=ORIENTED_EDGE('',*,*,#2254,.F.);
#2932=ORIENTED_EDGE('',*,*,#2255,.T.);
#2933=ORIENTED_EDGE('',*,*,#2256,.T.);
#2934=ORIENTED_EDGE('',*,*,#2255,.F.);
#2935=ORIENTED_EDGE('',*,*,#2254,.T.);
#2936=ORIENTED_EDGE('',*,*,#2251,.T.);
#2937=ORIENTED_EDGE('',*,*,#2256,.F.);
#2938=ORIENTED_EDGE('',*,*,#2253,.F.);
#2939=ORIENTED_EDGE('',*,*,#2257,.T.);
#2940=ORIENTED_EDGE('',*,*,#2258,.T.);
#2941=ORIENTED_EDGE('',*,*,#2259,.T.);
#2942=ORIENTED_EDGE('',*,*,#2260,.F.);
#2943=ORIENTED_EDGE('',*,*,#2261,.T.);
#2944=ORIENTED_EDGE('',*,*,#2262,.T.);
#2945=ORIENTED_EDGE('',*,*,#2263,.T.);
#2946=ORIENTED_EDGE('',*,*,#2258,.F.);
#2947=ORIENTED_EDGE('',*,*,#2264,.T.);
#2948=ORIENTED_EDGE('',*,*,#2265,.T.);
#2949=ORIENTED_EDGE('',*,*,#2266,.T.);
#2950=ORIENTED_EDGE('',*,*,#2262,.F.);
#2951=ORIENTED_EDGE('',*,*,#2267,.T.);
#2952=ORIENTED_EDGE('',*,*,#2268,.T.);
#2953=ORIENTED_EDGE('',*,*,#2269,.T.);
#2954=ORIENTED_EDGE('',*,*,#2265,.F.);
#2955=ORIENTED_EDGE('',*,*,#2270,.T.);
#2956=ORIENTED_EDGE('',*,*,#2271,.T.);
#2957=ORIENTED_EDGE('',*,*,#2272,.T.);
#2958=ORIENTED_EDGE('',*,*,#2268,.F.);
#2959=ORIENTED_EDGE('',*,*,#2273,.T.);
#2960=ORIENTED_EDGE('',*,*,#2260,.T.);
#2961=ORIENTED_EDGE('',*,*,#2274,.T.);
#2962=ORIENTED_EDGE('',*,*,#2271,.F.);
#2963=ORIENTED_EDGE('',*,*,#2273,.F.);
#2964=ORIENTED_EDGE('',*,*,#2270,.F.);
#2965=ORIENTED_EDGE('',*,*,#2267,.F.);
#2966=ORIENTED_EDGE('',*,*,#2264,.F.);
#2967=ORIENTED_EDGE('',*,*,#2261,.F.);
#2968=ORIENTED_EDGE('',*,*,#2257,.F.);
#2969=ORIENTED_EDGE('',*,*,#2274,.F.);
#2970=ORIENTED_EDGE('',*,*,#2259,.F.);
#2971=ORIENTED_EDGE('',*,*,#2263,.F.);
#2972=ORIENTED_EDGE('',*,*,#2266,.F.);
#2973=ORIENTED_EDGE('',*,*,#2269,.F.);
#2974=ORIENTED_EDGE('',*,*,#2272,.F.);
#2975=ORIENTED_EDGE('',*,*,#2275,.F.);
#2976=ORIENTED_EDGE('',*,*,#2276,.F.);
#2977=ORIENTED_EDGE('',*,*,#2277,.F.);
#2978=ORIENTED_EDGE('',*,*,#2278,.T.);
#2979=ORIENTED_EDGE('',*,*,#2276,.T.);
#2980=ORIENTED_EDGE('',*,*,#2278,.F.);
#2981=ORIENTED_EDGE('',*,*,#2279,.F.);
#2982=ORIENTED_EDGE('',*,*,#2280,.T.);
#2983=ORIENTED_EDGE('',*,*,#2277,.T.);
#2984=ORIENTED_EDGE('',*,*,#2280,.F.);
#2985=ORIENTED_EDGE('',*,*,#2281,.F.);
#2986=ORIENTED_EDGE('',*,*,#2282,.T.);
#2987=ORIENTED_EDGE('',*,*,#2279,.T.);
#2988=ORIENTED_EDGE('',*,*,#2282,.F.);
#2989=ORIENTED_EDGE('',*,*,#2281,.T.);
#2990=ORIENTED_EDGE('',*,*,#2283,.F.);
#2991=ORIENTED_EDGE('',*,*,#2284,.F.);
#2992=ORIENTED_EDGE('',*,*,#2285,.T.);
#2993=ORIENTED_EDGE('',*,*,#2283,.T.);
#2994=ORIENTED_EDGE('',*,*,#2285,.F.);
#2995=ORIENTED_EDGE('',*,*,#2275,.T.);
#2996=ORIENTED_EDGE('',*,*,#2286,.T.);
#2997=ORIENTED_EDGE('',*,*,#2284,.T.);
#2998=ORIENTED_EDGE('',*,*,#2286,.F.);
#2999=ORIENTED_EDGE('',*,*,#2287,.T.);
#3000=ORIENTED_EDGE('',*,*,#2288,.T.);
#3001=ORIENTED_EDGE('',*,*,#2289,.T.);
#3002=ORIENTED_EDGE('',*,*,#2290,.F.);
#3003=ORIENTED_EDGE('',*,*,#2291,.T.);
#3004=ORIENTED_EDGE('',*,*,#2292,.T.);
#3005=ORIENTED_EDGE('',*,*,#2293,.T.);
#3006=ORIENTED_EDGE('',*,*,#2288,.F.);
#3007=ORIENTED_EDGE('',*,*,#2294,.T.);
#3008=ORIENTED_EDGE('',*,*,#2295,.T.);
#3009=ORIENTED_EDGE('',*,*,#2296,.T.);
#3010=ORIENTED_EDGE('',*,*,#2292,.F.);
#3011=ORIENTED_EDGE('',*,*,#2297,.T.);
#3012=ORIENTED_EDGE('',*,*,#2298,.T.);
#3013=ORIENTED_EDGE('',*,*,#2299,.T.);
#3014=ORIENTED_EDGE('',*,*,#2295,.F.);
#3015=ORIENTED_EDGE('',*,*,#2300,.T.);
#3016=ORIENTED_EDGE('',*,*,#2301,.T.);
#3017=ORIENTED_EDGE('',*,*,#2302,.T.);
#3018=ORIENTED_EDGE('',*,*,#2298,.F.);
#3019=ORIENTED_EDGE('',*,*,#2303,.T.);
#3020=ORIENTED_EDGE('',*,*,#2290,.T.);
#3021=ORIENTED_EDGE('',*,*,#2304,.T.);
#3022=ORIENTED_EDGE('',*,*,#2301,.F.);
#3023=ORIENTED_EDGE('',*,*,#2303,.F.);
#3024=ORIENTED_EDGE('',*,*,#2300,.F.);
#3025=ORIENTED_EDGE('',*,*,#2297,.F.);
#3026=ORIENTED_EDGE('',*,*,#2294,.F.);
#3027=ORIENTED_EDGE('',*,*,#2291,.F.);
#3028=ORIENTED_EDGE('',*,*,#2287,.F.);
#3029=ORIENTED_EDGE('',*,*,#2304,.F.);
#3030=ORIENTED_EDGE('',*,*,#2289,.F.);
#3031=ORIENTED_EDGE('',*,*,#2293,.F.);
#3032=ORIENTED_EDGE('',*,*,#2296,.F.);
#3033=ORIENTED_EDGE('',*,*,#2299,.F.);
#3034=ORIENTED_EDGE('',*,*,#2302,.F.);
#3035=ORIENTED_EDGE('',*,*,#2305,.F.);
#3036=ORIENTED_EDGE('',*,*,#2306,.F.);
#3037=ORIENTED_EDGE('',*,*,#2307,.F.);
#3038=ORIENTED_EDGE('',*,*,#2308,.T.);
#3039=ORIENTED_EDGE('',*,*,#2306,.T.);
#3040=ORIENTED_EDGE('',*,*,#2308,.F.);
#3041=ORIENTED_EDGE('',*,*,#2309,.F.);
#3042=ORIENTED_EDGE('',*,*,#2310,.T.);
#3043=ORIENTED_EDGE('',*,*,#2307,.T.);
#3044=ORIENTED_EDGE('',*,*,#2310,.F.);
#3045=ORIENTED_EDGE('',*,*,#2311,.F.);
#3046=ORIENTED_EDGE('',*,*,#2312,.T.);
#3047=ORIENTED_EDGE('',*,*,#2309,.T.);
#3048=ORIENTED_EDGE('',*,*,#2312,.F.);
#3049=ORIENTED_EDGE('',*,*,#2311,.T.);
#3050=ORIENTED_EDGE('',*,*,#2313,.F.);
#3051=ORIENTED_EDGE('',*,*,#2314,.F.);
#3052=ORIENTED_EDGE('',*,*,#2315,.T.);
#3053=ORIENTED_EDGE('',*,*,#2313,.T.);
#3054=ORIENTED_EDGE('',*,*,#2315,.F.);
#3055=ORIENTED_EDGE('',*,*,#2305,.T.);
#3056=ORIENTED_EDGE('',*,*,#2316,.T.);
#3057=ORIENTED_EDGE('',*,*,#2314,.T.);
#3058=ORIENTED_EDGE('',*,*,#2316,.F.);
#3059=ORIENTED_EDGE('',*,*,#2317,.F.);
#3060=ORIENTED_EDGE('',*,*,#2318,.T.);
#3061=ORIENTED_EDGE('',*,*,#2319,.F.);
#3062=ORIENTED_EDGE('',*,*,#2318,.F.);
#3063=ORIENTED_EDGE('',*,*,#2320,.F.);
#3064=ORIENTED_EDGE('',*,*,#2321,.T.);
#3065=ORIENTED_EDGE('',*,*,#2322,.F.);
#3066=ORIENTED_EDGE('',*,*,#2321,.F.);
#3067=ORIENTED_EDGE('',*,*,#2323,.F.);
#3068=ORIENTED_EDGE('',*,*,#2324,.T.);
#3069=ORIENTED_EDGE('',*,*,#2325,.F.);
#3070=ORIENTED_EDGE('',*,*,#2324,.F.);
#3071=ORIENTED_EDGE('',*,*,#2326,.F.);
#3072=ORIENTED_EDGE('',*,*,#2327,.T.);
#3073=ORIENTED_EDGE('',*,*,#2328,.F.);
#3074=ORIENTED_EDGE('',*,*,#2327,.F.);
#3075=ORIENTED_EDGE('',*,*,#2329,.F.);
#3076=ORIENTED_EDGE('',*,*,#2330,.F.);
#3077=ORIENTED_EDGE('',*,*,#2331,.F.);
#3078=ORIENTED_EDGE('',*,*,#2332,.F.);
#3079=ORIENTED_EDGE('',*,*,#2333,.F.);
#3080=ORIENTED_EDGE('',*,*,#2334,.F.);
#3081=ORIENTED_EDGE('',*,*,#2330,.T.);
#3082=ORIENTED_EDGE('',*,*,#2335,.T.);
#3083=ORIENTED_EDGE('',*,*,#2336,.F.);
#3084=ORIENTED_EDGE('',*,*,#2337,.T.);
#3085=ORIENTED_EDGE('',*,*,#2338,.T.);
#3086=ORIENTED_EDGE('',*,*,#2339,.F.);
#3087=ORIENTED_EDGE('',*,*,#2336,.T.);
#3088=ORIENTED_EDGE('',*,*,#2340,.T.);
#3089=ORIENTED_EDGE('',*,*,#2340,.F.);
#3090=ORIENTED_EDGE('',*,*,#2341,.T.);
#3091=ORIENTED_EDGE('',*,*,#2333,.T.);
#3092=ORIENTED_EDGE('',*,*,#2341,.F.);
#3093=ORIENTED_EDGE('',*,*,#2342,.T.);
#3094=ORIENTED_EDGE('',*,*,#2337,.F.);
#3095=ORIENTED_EDGE('',*,*,#2335,.F.);
#3096=ORIENTED_EDGE('',*,*,#2329,.T.);
#3097=ORIENTED_EDGE('',*,*,#2331,.T.);
#3098=ORIENTED_EDGE('',*,*,#2334,.T.);
#3099=ORIENTED_EDGE('',*,*,#2339,.T.);
#3100=ORIENTED_EDGE('',*,*,#2343,.T.);
#3101=ORIENTED_EDGE('',*,*,#2344,.T.);
#3102=ORIENTED_EDGE('',*,*,#2345,.F.);
#3103=ORIENTED_EDGE('',*,*,#2346,.T.);
#3104=ORIENTED_EDGE('',*,*,#2347,.T.);
#3105=ORIENTED_EDGE('',*,*,#2348,.F.);
#3106=ORIENTED_EDGE('',*,*,#2349,.T.);
#3107=ORIENTED_EDGE('',*,*,#2350,.F.);
#3108=ORIENTED_EDGE('',*,*,#2344,.F.);
#3109=ORIENTED_EDGE('',*,*,#2351,.F.);
#3110=ORIENTED_EDGE('',*,*,#2352,.T.);
#3111=ORIENTED_EDGE('',*,*,#2353,.F.);
#3112=ORIENTED_EDGE('',*,*,#2349,.F.);
#3113=ORIENTED_EDGE('',*,*,#2354,.F.);
#3114=ORIENTED_EDGE('',*,*,#2355,.F.);
#3115=ORIENTED_EDGE('',*,*,#2356,.F.);
#3116=ORIENTED_EDGE('',*,*,#2352,.F.);
#3117=ORIENTED_EDGE('',*,*,#2347,.F.);
#3118=ORIENTED_EDGE('',*,*,#2357,.T.);
#3119=ORIENTED_EDGE('',*,*,#2358,.T.);
#3120=ORIENTED_EDGE('',*,*,#2359,.T.);
#3121=ORIENTED_EDGE('',*,*,#2360,.F.);
#3122=ORIENTED_EDGE('',*,*,#2361,.F.);
#3123=ORIENTED_EDGE('',*,*,#2362,.F.);
#3124=ORIENTED_EDGE('',*,*,#2363,.F.);
#3125=ORIENTED_EDGE('',*,*,#2364,.F.);
#3126=ORIENTED_EDGE('',*,*,#2354,.T.);
#3127=ORIENTED_EDGE('',*,*,#2351,.T.);
#3128=ORIENTED_EDGE('',*,*,#2348,.T.);
#3129=ORIENTED_EDGE('',*,*,#2343,.F.);
#3130=ORIENTED_EDGE('',*,*,#2338,.F.);
#3131=ORIENTED_EDGE('',*,*,#2342,.F.);
#3132=ORIENTED_EDGE('',*,*,#2332,.T.);
#3133=ORIENTED_EDGE('',*,*,#2317,.T.);
#3134=ORIENTED_EDGE('',*,*,#2320,.T.);
#3135=ORIENTED_EDGE('',*,*,#2323,.T.);
#3136=ORIENTED_EDGE('',*,*,#2326,.T.);
#3137=ORIENTED_EDGE('',*,*,#2365,.F.);
#3138=ORIENTED_EDGE('',*,*,#2366,.F.);
#3139=ORIENTED_EDGE('',*,*,#2357,.F.);
#3140=ORIENTED_EDGE('',*,*,#2346,.F.);
#3141=ORIENTED_EDGE('',*,*,#2367,.F.);
#3142=ORIENTED_EDGE('',*,*,#2368,.F.);
#3143=ORIENTED_EDGE('',*,*,#2358,.F.);
#3144=ORIENTED_EDGE('',*,*,#2366,.T.);
#3145=ORIENTED_EDGE('',*,*,#2369,.F.);
#3146=ORIENTED_EDGE('',*,*,#2370,.F.);
#3147=ORIENTED_EDGE('',*,*,#2359,.F.);
#3148=ORIENTED_EDGE('',*,*,#2368,.T.);
#3149=ORIENTED_EDGE('',*,*,#2370,.T.);
#3150=ORIENTED_EDGE('',*,*,#2371,.F.);
#3151=ORIENTED_EDGE('',*,*,#2372,.F.);
#3152=ORIENTED_EDGE('',*,*,#2360,.T.);
#3153=ORIENTED_EDGE('',*,*,#2355,.T.);
#3154=ORIENTED_EDGE('',*,*,#2364,.T.);
#3155=ORIENTED_EDGE('',*,*,#2373,.T.);
#3156=ORIENTED_EDGE('',*,*,#2374,.F.);
#3157=ORIENTED_EDGE('',*,*,#2362,.T.);
#3158=ORIENTED_EDGE('',*,*,#2375,.T.);
#3159=ORIENTED_EDGE('',*,*,#2376,.F.);
#3160=ORIENTED_EDGE('',*,*,#2377,.F.);
#3161=ORIENTED_EDGE('',*,*,#2363,.T.);
#3162=ORIENTED_EDGE('',*,*,#2377,.T.);
#3163=ORIENTED_EDGE('',*,*,#2378,.F.);
#3164=ORIENTED_EDGE('',*,*,#2373,.F.);
#3165=ORIENTED_EDGE('',*,*,#2361,.T.);
#3166=ORIENTED_EDGE('',*,*,#2372,.T.);
#3167=ORIENTED_EDGE('',*,*,#2379,.F.);
#3168=ORIENTED_EDGE('',*,*,#2375,.F.);
#3169=ORIENTED_EDGE('',*,*,#2356,.T.);
#3170=ORIENTED_EDGE('',*,*,#2374,.T.);
#3171=ORIENTED_EDGE('',*,*,#2378,.T.);
#3172=ORIENTED_EDGE('',*,*,#2376,.T.);
#3173=ORIENTED_EDGE('',*,*,#2379,.T.);
#3174=ORIENTED_EDGE('',*,*,#2371,.T.);
#3175=ORIENTED_EDGE('',*,*,#2369,.T.);
#3176=ORIENTED_EDGE('',*,*,#2367,.T.);
#3177=ORIENTED_EDGE('',*,*,#2365,.T.);
#3178=ORIENTED_EDGE('',*,*,#2345,.T.);
#3179=ORIENTED_EDGE('',*,*,#2350,.T.);
#3180=ORIENTED_EDGE('',*,*,#2353,.T.);
#3181=ORIENTED_EDGE('',*,*,#2319,.T.);
#3182=ORIENTED_EDGE('',*,*,#2322,.T.);
#3183=ORIENTED_EDGE('',*,*,#2325,.T.);
#3184=ORIENTED_EDGE('',*,*,#2328,.T.);
#3185=ORIENTED_EDGE('',*,*,#2380,.F.);
#3186=ORIENTED_EDGE('',*,*,#2381,.T.);
#3187=ORIENTED_EDGE('',*,*,#2382,.F.);
#3188=ORIENTED_EDGE('',*,*,#2383,.T.);
#3189=ORIENTED_EDGE('',*,*,#2380,.T.);
#3190=ORIENTED_EDGE('',*,*,#2383,.F.);
#3191=ORIENTED_EDGE('',*,*,#2382,.T.);
#3192=ORIENTED_EDGE('',*,*,#2384,.T.);
#3193=ORIENTED_EDGE('',*,*,#2384,.F.);
#3194=ORIENTED_EDGE('',*,*,#2385,.T.);
#3195=ORIENTED_EDGE('',*,*,#2386,.T.);
#3196=ORIENTED_EDGE('',*,*,#2385,.F.);
#3197=ORIENTED_EDGE('',*,*,#2381,.F.);
#3198=ORIENTED_EDGE('',*,*,#2387,.T.);
#3199=ORIENTED_EDGE('',*,*,#2388,.T.);
#3200=ORIENTED_EDGE('',*,*,#2387,.F.);
#3201=ORIENTED_EDGE('',*,*,#2388,.F.);
#3202=ORIENTED_EDGE('',*,*,#2386,.F.);
#3203=ORIENTED_EDGE('',*,*,#2389,.F.);
#3204=ORIENTED_EDGE('',*,*,#2390,.T.);
#3205=ORIENTED_EDGE('',*,*,#2391,.F.);
#3206=ORIENTED_EDGE('',*,*,#2392,.T.);
#3207=ORIENTED_EDGE('',*,*,#2389,.T.);
#3208=ORIENTED_EDGE('',*,*,#2392,.F.);
#3209=ORIENTED_EDGE('',*,*,#2391,.T.);
#3210=ORIENTED_EDGE('',*,*,#2393,.T.);
#3211=ORIENTED_EDGE('',*,*,#2393,.F.);
#3212=ORIENTED_EDGE('',*,*,#2394,.T.);
#3213=ORIENTED_EDGE('',*,*,#2395,.T.);
#3214=ORIENTED_EDGE('',*,*,#2394,.F.);
#3215=ORIENTED_EDGE('',*,*,#2390,.F.);
#3216=ORIENTED_EDGE('',*,*,#2396,.T.);
#3217=ORIENTED_EDGE('',*,*,#2397,.T.);
#3218=ORIENTED_EDGE('',*,*,#2396,.F.);
#3219=ORIENTED_EDGE('',*,*,#2397,.F.);
#3220=ORIENTED_EDGE('',*,*,#2395,.F.);
#3221=ORIENTED_EDGE('',*,*,#2398,.F.);
#3222=ORIENTED_EDGE('',*,*,#2399,.T.);
#3223=ORIENTED_EDGE('',*,*,#2400,.F.);
#3224=ORIENTED_EDGE('',*,*,#2401,.T.);
#3225=ORIENTED_EDGE('',*,*,#2398,.T.);
#3226=ORIENTED_EDGE('',*,*,#2401,.F.);
#3227=ORIENTED_EDGE('',*,*,#2400,.T.);
#3228=ORIENTED_EDGE('',*,*,#2402,.T.);
#3229=ORIENTED_EDGE('',*,*,#2402,.F.);
#3230=ORIENTED_EDGE('',*,*,#2403,.T.);
#3231=ORIENTED_EDGE('',*,*,#2404,.T.);
#3232=ORIENTED_EDGE('',*,*,#2403,.F.);
#3233=ORIENTED_EDGE('',*,*,#2399,.F.);
#3234=ORIENTED_EDGE('',*,*,#2405,.T.);
#3235=ORIENTED_EDGE('',*,*,#2406,.T.);
#3236=ORIENTED_EDGE('',*,*,#2405,.F.);
#3237=ORIENTED_EDGE('',*,*,#2406,.F.);
#3238=ORIENTED_EDGE('',*,*,#2404,.F.);
#3239=ORIENTED_EDGE('',*,*,#2407,.F.);
#3240=ORIENTED_EDGE('',*,*,#2408,.T.);
#3241=ORIENTED_EDGE('',*,*,#2409,.F.);
#3242=ORIENTED_EDGE('',*,*,#2410,.T.);
#3243=ORIENTED_EDGE('',*,*,#2407,.T.);
#3244=ORIENTED_EDGE('',*,*,#2410,.F.);
#3245=ORIENTED_EDGE('',*,*,#2409,.T.);
#3246=ORIENTED_EDGE('',*,*,#2411,.T.);
#3247=ORIENTED_EDGE('',*,*,#2411,.F.);
#3248=ORIENTED_EDGE('',*,*,#2412,.T.);
#3249=ORIENTED_EDGE('',*,*,#2413,.T.);
#3250=ORIENTED_EDGE('',*,*,#2412,.F.);
#3251=ORIENTED_EDGE('',*,*,#2408,.F.);
#3252=ORIENTED_EDGE('',*,*,#2414,.T.);
#3253=ORIENTED_EDGE('',*,*,#2415,.T.);
#3254=ORIENTED_EDGE('',*,*,#2414,.F.);
#3255=ORIENTED_EDGE('',*,*,#2415,.F.);
#3256=ORIENTED_EDGE('',*,*,#2413,.F.);
#3257=ORIENTED_EDGE('',*,*,#2416,.F.);
#3258=ORIENTED_EDGE('',*,*,#2417,.T.);
#3259=ORIENTED_EDGE('',*,*,#2418,.F.);
#3260=ORIENTED_EDGE('',*,*,#2417,.F.);
#3261=ORIENTED_EDGE('',*,*,#2419,.F.);
#3262=ORIENTED_EDGE('',*,*,#2420,.T.);
#3263=ORIENTED_EDGE('',*,*,#2421,.T.);
#3264=ORIENTED_EDGE('',*,*,#2422,.F.);
#3265=ORIENTED_EDGE('',*,*,#2423,.T.);
#3266=ORIENTED_EDGE('',*,*,#2424,.T.);
#3267=ORIENTED_EDGE('',*,*,#2425,.F.);
#3268=ORIENTED_EDGE('',*,*,#2421,.F.);
#3269=ORIENTED_EDGE('',*,*,#2426,.F.);
#3270=ORIENTED_EDGE('',*,*,#2427,.F.);
#3271=ORIENTED_EDGE('',*,*,#2424,.F.);
#3272=ORIENTED_EDGE('',*,*,#2428,.T.);
#3273=ORIENTED_EDGE('',*,*,#2429,.T.);
#3274=ORIENTED_EDGE('',*,*,#2422,.T.);
#3275=ORIENTED_EDGE('',*,*,#2425,.T.);
#3276=ORIENTED_EDGE('',*,*,#2427,.T.);
#3277=ORIENTED_EDGE('',*,*,#2418,.T.);
#3278=ORIENTED_EDGE('',*,*,#2430,.F.);
#3279=ORIENTED_EDGE('',*,*,#2428,.F.);
#3280=ORIENTED_EDGE('',*,*,#2423,.F.);
#3281=ORIENTED_EDGE('',*,*,#2420,.F.);
#3282=ORIENTED_EDGE('',*,*,#2431,.T.);
#3283=ORIENTED_EDGE('',*,*,#2419,.T.);
#3284=ORIENTED_EDGE('',*,*,#2429,.F.);
#3285=ORIENTED_EDGE('',*,*,#2426,.T.);
#3286=ORIENTED_EDGE('',*,*,#2430,.T.);
#3287=ORIENTED_EDGE('',*,*,#2431,.F.);
#3288=ORIENTED_EDGE('',*,*,#2432,.T.);
#3289=ORIENTED_EDGE('',*,*,#2433,.T.);
#3290=ORIENTED_EDGE('',*,*,#2432,.F.);
#3291=ORIENTED_EDGE('',*,*,#2433,.F.);
#3292=ORIENTED_EDGE('',*,*,#2416,.T.);
#3293=ORIENTED_EDGE('',*,*,#2434,.F.);
#3294=ORIENTED_EDGE('',*,*,#2435,.T.);
#3295=ORIENTED_EDGE('',*,*,#2436,.T.);
#3296=ORIENTED_EDGE('',*,*,#2435,.F.);
#3297=ORIENTED_EDGE('',*,*,#2434,.T.);
#3298=ORIENTED_EDGE('',*,*,#2436,.F.);
#3299=CYLINDRICAL_SURFACE('',#3884,0.164999999999999);
#3300=CYLINDRICAL_SURFACE('',#3887,0.164999999999999);
#3301=CYLINDRICAL_SURFACE('',#3890,0.21);
#3302=CYLINDRICAL_SURFACE('',#3893,0.21);
#3303=CYLINDRICAL_SURFACE('',#3896,0.21);
#3304=CYLINDRICAL_SURFACE('',#3899,0.21);
#3305=CYLINDRICAL_SURFACE('',#3902,0.21);
#3306=CYLINDRICAL_SURFACE('',#3905,0.21);
#3307=CYLINDRICAL_SURFACE('',#3908,0.21);
#3308=CYLINDRICAL_SURFACE('',#3911,0.21);
#3309=CYLINDRICAL_SURFACE('',#3914,0.21);
#3310=CYLINDRICAL_SURFACE('',#3917,0.21);
#3311=CYLINDRICAL_SURFACE('',#3920,0.21);
#3312=CYLINDRICAL_SURFACE('',#3923,0.21);
#3313=CYLINDRICAL_SURFACE('',#3933,0.800000000000001);
#3314=CYLINDRICAL_SURFACE('',#3939,0.800000000000001);
#3315=CYLINDRICAL_SURFACE('',#3945,0.800000000000001);
#3316=CYLINDRICAL_SURFACE('',#3951,0.800000000000001);
#3317=CYLINDRICAL_SURFACE('',#3957,0.45);
#3318=CYLINDRICAL_SURFACE('',#3962,0.45);
#3319=CYLINDRICAL_SURFACE('',#3967,0.45);
#3320=CYLINDRICAL_SURFACE('',#3972,0.45);
#3321=CYLINDRICAL_SURFACE('',#3977,0.275);
#3322=CYLINDRICAL_SURFACE('',#3979,0.275);
#3323=CYLINDRICAL_SURFACE('',#3981,0.275);
#3324=CYLINDRICAL_SURFACE('',#3983,0.275);
#3325=CYLINDRICAL_SURFACE('',#4004,0.475);
#3326=CYLINDRICAL_SURFACE('',#4009,0.275);
#3327=CYLINDRICAL_SURFACE('',#4011,0.275);
#3328=CYLINDRICAL_SURFACE('',#4014,0.405);
#3329=CYLINDRICAL_SURFACE('',#4026,0.475);
#3330=CYLINDRICAL_SURFACE('',#4031,0.275);
#3331=CYLINDRICAL_SURFACE('',#4033,0.275);
#3332=CYLINDRICAL_SURFACE('',#4036,0.405);
#3333=CYLINDRICAL_SURFACE('',#4048,0.165);
#3334=CYLINDRICAL_SURFACE('',#4052,0.165);
#3335=CYLINDRICAL_SURFACE('',#4056,0.4);
#3336=CYLINDRICAL_SURFACE('',#4062,0.225);
#3337=CYLINDRICAL_SURFACE('',#4065,0.8);
#3338=CYLINDRICAL_SURFACE('',#4071,0.225);
#3339=CYLINDRICAL_SURFACE('',#4074,0.8);
#3340=CYLINDRICAL_SURFACE('',#4080,0.164999999999999);
#3341=CYLINDRICAL_SURFACE('',#4087,0.225);
#3342=CYLINDRICAL_SURFACE('',#4094,0.225);
#3343=CYLINDRICAL_SURFACE('',#4098,0.6);
#3344=CYLINDRICAL_SURFACE('',#4105,1.2);
#3345=CYLINDRICAL_SURFACE('',#4107,0.300000000000001);
#3346=CYLINDRICAL_SURFACE('',#4114,0.305);
#3347=CYLINDRICAL_SURFACE('',#4117,0.5);
#3348=CYLINDRICAL_SURFACE('',#4123,0.225);
#3349=CYLINDRICAL_SURFACE('',#4126,0.6);
#3350=CYLINDRICAL_SURFACE('',#4146,0.425);
#3351=CYLINDRICAL_SURFACE('',#4154,0.24505);
#3352=CYLINDRICAL_SURFACE('',#4170,0.35);
#3353=CYLINDRICAL_SURFACE('',#4178,0.1954);
#3354=CYLINDRICAL_SURFACE('',#4209,0.7);
#3355=CYLINDRICAL_SURFACE('',#4212,0.7);
#3356=CYLINDRICAL_SURFACE('',#4215,0.6);
#3357=CYLINDRICAL_SURFACE('',#4218,0.6);
#3358=CYLINDRICAL_SURFACE('',#4228,0.405);
#3359=CYLINDRICAL_SURFACE('',#4229,0.8);
#3360=CYLINDRICAL_SURFACE('',#4248,0.8);
#3361=CYLINDRICAL_SURFACE('',#4252,0.4);
#3362=CYLINDRICAL_SURFACE('',#4254,0.6);
#3363=CYLINDRICAL_SURFACE('',#4261,0.8);
#3364=CYLINDRICAL_SURFACE('',#4265,0.4);
#3365=CYLINDRICAL_SURFACE('',#4267,0.6);
#3366=CYLINDRICAL_SURFACE('',#4274,0.9);
#3367=CYLINDRICAL_SURFACE('',#4278,0.5);
#3368=CYLINDRICAL_SURFACE('',#4280,0.7);
#3369=CYLINDRICAL_SURFACE('',#4287,0.9);
#3370=CYLINDRICAL_SURFACE('',#4291,0.5);
#3371=CYLINDRICAL_SURFACE('',#4293,0.7);
#3372=CYLINDRICAL_SURFACE('',#4303,0.305);
#3373=CYLINDRICAL_SURFACE('',#4314,1.4);
#3374=CYLINDRICAL_SURFACE('',#4315,1.);
#3375=CYLINDRICAL_SURFACE('',#4319,0.6);
#3376=ADVANCED_FACE('',(#501),#3299,.F.);
#3377=ADVANCED_FACE('',(#502),#3300,.F.);
#3378=ADVANCED_FACE('',(#503),#3301,.F.);
#3379=ADVANCED_FACE('',(#504),#3302,.F.);
#3380=ADVANCED_FACE('',(#505),#3303,.F.);
#3381=ADVANCED_FACE('',(#506),#3304,.F.);
#3382=ADVANCED_FACE('',(#507),#3305,.F.);
#3383=ADVANCED_FACE('',(#508),#3306,.F.);
#3384=ADVANCED_FACE('',(#509),#3307,.F.);
#3385=ADVANCED_FACE('',(#510),#3308,.F.);
#3386=ADVANCED_FACE('',(#511),#3309,.F.);
#3387=ADVANCED_FACE('',(#512),#3310,.F.);
#3388=ADVANCED_FACE('',(#513),#3311,.F.);
#3389=ADVANCED_FACE('',(#514),#3312,.F.);
#3390=ADVANCED_FACE('',(#515),#370,.T.);
#3391=ADVANCED_FACE('',(#516),#371,.T.);
#3392=ADVANCED_FACE('',(#517),#372,.T.);
#3393=ADVANCED_FACE('',(#518),#373,.T.);
#3394=ADVANCED_FACE('',(#519,#269,#270,#271,#272,#273,#274,#275,#276,#277,
#278,#279,#280,#281,#282),#374,.T.);
#3395=ADVANCED_FACE('',(#520,#283,#284,#285,#286,#287,#288,#289,#290,#291,
#292,#293,#294,#295,#296),#375,.F.);
#3396=ADVANCED_FACE('',(#521),#3313,.T.);
#3397=ADVANCED_FACE('',(#522),#376,.T.);
#3398=ADVANCED_FACE('',(#523),#377,.F.);
#3399=ADVANCED_FACE('',(#524),#3314,.T.);
#3400=ADVANCED_FACE('',(#525),#378,.T.);
#3401=ADVANCED_FACE('',(#526),#379,.F.);
#3402=ADVANCED_FACE('',(#527),#3315,.T.);
#3403=ADVANCED_FACE('',(#528),#380,.T.);
#3404=ADVANCED_FACE('',(#529),#381,.F.);
#3405=ADVANCED_FACE('',(#530),#3316,.T.);
#3406=ADVANCED_FACE('',(#531),#382,.T.);
#3407=ADVANCED_FACE('',(#532),#383,.F.);
#3408=ADVANCED_FACE('',(#533),#3317,.F.);
#3409=ADVANCED_FACE('',(#534,#297),#384,.T.);
#3410=ADVANCED_FACE('',(#535),#3318,.F.);
#3411=ADVANCED_FACE('',(#536,#298),#385,.T.);
#3412=ADVANCED_FACE('',(#537),#3319,.F.);
#3413=ADVANCED_FACE('',(#538,#299),#386,.T.);
#3414=ADVANCED_FACE('',(#539),#3320,.F.);
#3415=ADVANCED_FACE('',(#540,#300),#387,.T.);
#3416=ADVANCED_FACE('',(#541),#3321,.F.);
#3417=ADVANCED_FACE('',(#542),#3322,.F.);
#3418=ADVANCED_FACE('',(#543),#3323,.F.);
#3419=ADVANCED_FACE('',(#544),#3324,.F.);
#3420=ADVANCED_FACE('',(#545),#388,.F.);
#3421=ADVANCED_FACE('',(#546),#389,.F.);
#3422=ADVANCED_FACE('',(#547),#390,.F.);
#3423=ADVANCED_FACE('',(#548),#391,.F.);
#3424=ADVANCED_FACE('',(#549),#392,.T.);
#3425=ADVANCED_FACE('',(#550),#393,.T.);
#3426=ADVANCED_FACE('',(#551),#394,.T.);
#3427=ADVANCED_FACE('',(#552),#395,.T.);
#3428=ADVANCED_FACE('',(#553),#396,.T.);
#3429=ADVANCED_FACE('',(#554,#301,#302,#303,#304,#305),#397,.T.);
#3430=ADVANCED_FACE('',(#555,#306,#307,#308,#309),#398,.F.);
#3431=ADVANCED_FACE('',(#556),#399,.T.);
#3432=ADVANCED_FACE('',(#557),#400,.T.);
#3433=ADVANCED_FACE('',(#558),#401,.T.);
#3434=ADVANCED_FACE('',(#559),#402,.T.);
#3435=ADVANCED_FACE('',(#560),#403,.T.);
#3436=ADVANCED_FACE('',(#561),#404,.F.);
#3437=ADVANCED_FACE('',(#562,#310),#3325,.F.);
#3438=ADVANCED_FACE('',(#563,#311),#405,.T.);
#3439=ADVANCED_FACE('',(#564),#3326,.F.);
#3440=ADVANCED_FACE('',(#565),#3327,.F.);
#3441=ADVANCED_FACE('',(#566,#312),#3328,.F.);
#3442=ADVANCED_FACE('',(#567,#313),#406,.T.);
#3443=ADVANCED_FACE('',(#568),#407,.T.);
#3444=ADVANCED_FACE('',(#569,#314),#408,.T.);
#3445=ADVANCED_FACE('',(#570),#409,.T.);
#3446=ADVANCED_FACE('',(#571,#315,#316),#410,.T.);
#3447=ADVANCED_FACE('',(#572),#411,.T.);
#3448=ADVANCED_FACE('',(#573,#317),#412,.T.);
#3449=ADVANCED_FACE('',(#574,#318),#413,.F.);
#3450=ADVANCED_FACE('',(#575,#319),#3329,.F.);
#3451=ADVANCED_FACE('',(#576,#320),#414,.T.);
#3452=ADVANCED_FACE('',(#577),#3330,.F.);
#3453=ADVANCED_FACE('',(#578),#3331,.F.);
#3454=ADVANCED_FACE('',(#579,#321),#3332,.F.);
#3455=ADVANCED_FACE('',(#580,#322),#415,.T.);
#3456=ADVANCED_FACE('',(#581),#416,.T.);
#3457=ADVANCED_FACE('',(#582,#323),#417,.T.);
#3458=ADVANCED_FACE('',(#583),#418,.T.);
#3459=ADVANCED_FACE('',(#584,#324,#325),#419,.T.);
#3460=ADVANCED_FACE('',(#585),#420,.T.);
#3461=ADVANCED_FACE('',(#586,#326),#421,.T.);
#3462=ADVANCED_FACE('',(#587,#327),#422,.F.);
#3463=ADVANCED_FACE('',(#588),#3333,.F.);
#3464=ADVANCED_FACE('',(#589),#423,.T.);
#3465=ADVANCED_FACE('',(#590),#3334,.F.);
#3466=ADVANCED_FACE('',(#591),#424,.F.);
#3467=ADVANCED_FACE('',(#592),#3335,.T.);
#3468=ADVANCED_FACE('',(#593,#328),#425,.T.);
#3469=ADVANCED_FACE('',(#594,#329),#426,.F.);
#3470=ADVANCED_FACE('',(#595),#3336,.F.);
#3471=ADVANCED_FACE('',(#596),#3337,.T.);
#3472=ADVANCED_FACE('',(#597,#330),#427,.T.);
#3473=ADVANCED_FACE('',(#598,#331),#428,.F.);
#3474=ADVANCED_FACE('',(#599),#3338,.F.);
#3475=ADVANCED_FACE('',(#600),#3339,.T.);
#3476=ADVANCED_FACE('',(#601,#332),#429,.T.);
#3477=ADVANCED_FACE('',(#602,#333),#430,.F.);
#3478=ADVANCED_FACE('',(#603),#3340,.F.);
#3479=ADVANCED_FACE('',(#604),#431,.T.);
#3480=ADVANCED_FACE('',(#605),#432,.F.);
#3481=ADVANCED_FACE('',(#606),#3341,.F.);
#3482=ADVANCED_FACE('',(#607),#433,.F.);
#3483=ADVANCED_FACE('',(#608),#3342,.F.);
#3484=ADVANCED_FACE('',(#609),#3343,.T.);
#3485=ADVANCED_FACE('',(#610,#334),#434,.T.);
#3486=ADVANCED_FACE('',(#611),#3344,.T.);
#3487=ADVANCED_FACE('',(#612),#3345,.T.);
#3488=ADVANCED_FACE('',(#613,#335),#435,.T.);
#3489=ADVANCED_FACE('',(#614,#336),#436,.T.);
#3490=ADVANCED_FACE('',(#615,#337,#338),#437,.F.);
#3491=ADVANCED_FACE('',(#616),#3346,.F.);
#3492=ADVANCED_FACE('',(#617),#3347,.T.);
#3493=ADVANCED_FACE('',(#618,#339),#438,.T.);
#3494=ADVANCED_FACE('',(#619,#340),#439,.F.);
#3495=ADVANCED_FACE('',(#620),#3348,.F.);
#3496=ADVANCED_FACE('',(#621),#3349,.T.);
#3497=ADVANCED_FACE('',(#622,#341),#440,.T.);
#3498=ADVANCED_FACE('',(#623,#342),#441,.F.);
#3499=ADVANCED_FACE('',(#624),#442,.F.);
#3500=ADVANCED_FACE('',(#625),#443,.F.);
#3501=ADVANCED_FACE('',(#626),#444,.F.);
#3502=ADVANCED_FACE('',(#627),#445,.F.);
#3503=ADVANCED_FACE('',(#628),#446,.F.);
#3504=ADVANCED_FACE('',(#629),#447,.F.);
#3505=ADVANCED_FACE('',(#630),#448,.F.);
#3506=ADVANCED_FACE('',(#631),#449,.F.);
#3507=ADVANCED_FACE('',(#632),#450,.F.);
#3508=ADVANCED_FACE('',(#633),#451,.T.);
#3509=ADVANCED_FACE('',(#634),#163,.T.);
#3510=ADVANCED_FACE('',(#635),#3350,.T.);
#3511=ADVANCED_FACE('',(#636),#164,.T.);
#3512=ADVANCED_FACE('',(#637,#343),#452,.T.);
#3513=ADVANCED_FACE('',(#638),#165,.T.);
#3514=ADVANCED_FACE('',(#639),#3351,.T.);
#3515=ADVANCED_FACE('',(#640),#453,.F.);
#3516=ADVANCED_FACE('',(#641),#454,.F.);
#3517=ADVANCED_FACE('',(#642),#455,.F.);
#3518=ADVANCED_FACE('',(#643),#456,.F.);
#3519=ADVANCED_FACE('',(#644),#457,.F.);
#3520=ADVANCED_FACE('',(#645),#458,.F.);
#3521=ADVANCED_FACE('',(#646),#459,.F.);
#3522=ADVANCED_FACE('',(#647),#460,.F.);
#3523=ADVANCED_FACE('',(#648),#461,.F.);
#3524=ADVANCED_FACE('',(#649),#462,.T.);
#3525=ADVANCED_FACE('',(#650),#166,.T.);
#3526=ADVANCED_FACE('',(#651),#3352,.T.);
#3527=ADVANCED_FACE('',(#652),#167,.T.);
#3528=ADVANCED_FACE('',(#653,#344),#463,.T.);
#3529=ADVANCED_FACE('',(#654),#168,.T.);
#3530=ADVANCED_FACE('',(#655),#3353,.T.);
#3531=ADVANCED_FACE('',(#656),#3354,.F.);
#3532=ADVANCED_FACE('',(#657),#3355,.F.);
#3533=ADVANCED_FACE('',(#658),#3356,.F.);
#3534=ADVANCED_FACE('',(#659),#3357,.F.);
#3535=ADVANCED_FACE('',(#660,#345),#464,.F.);
#3536=ADVANCED_FACE('',(#661),#465,.T.);
#3537=ADVANCED_FACE('',(#662,#346),#466,.T.);
#3538=ADVANCED_FACE('',(#663),#3358,.F.);
#3539=ADVANCED_FACE('',(#664),#3359,.T.);
#3540=ADVANCED_FACE('',(#665),#467,.T.);
#3541=ADVANCED_FACE('',(#666),#468,.F.);
#3542=ADVANCED_FACE('',(#667),#469,.F.);
#3543=ADVANCED_FACE('',(#668),#470,.F.);
#3544=ADVANCED_FACE('',(#669,#347,#348,#349,#350),#471,.F.);
#3545=ADVANCED_FACE('',(#670),#472,.F.);
#3546=ADVANCED_FACE('',(#671),#473,.F.);
#3547=ADVANCED_FACE('',(#672),#474,.F.);
#3548=ADVANCED_FACE('',(#673),#475,.T.);
#3549=ADVANCED_FACE('',(#674),#476,.T.);
#3550=ADVANCED_FACE('',(#675),#477,.T.);
#3551=ADVANCED_FACE('',(#676),#478,.T.);
#3552=ADVANCED_FACE('',(#677),#479,.T.);
#3553=ADVANCED_FACE('',(#678,#351,#352,#353,#354),#480,.T.);
#3554=ADVANCED_FACE('',(#679,#355),#481,.F.);
#3555=ADVANCED_FACE('',(#680),#3360,.T.);
#3556=ADVANCED_FACE('',(#681,#356),#482,.T.);
#3557=ADVANCED_FACE('',(#682),#3361,.F.);
#3558=ADVANCED_FACE('',(#683),#3362,.T.);
#3559=ADVANCED_FACE('',(#684,#357),#483,.F.);
#3560=ADVANCED_FACE('',(#685,#358),#484,.F.);
#3561=ADVANCED_FACE('',(#686),#3363,.T.);
#3562=ADVANCED_FACE('',(#687,#359),#485,.T.);
#3563=ADVANCED_FACE('',(#688),#3364,.F.);
#3564=ADVANCED_FACE('',(#689),#3365,.T.);
#3565=ADVANCED_FACE('',(#690,#360),#486,.F.);
#3566=ADVANCED_FACE('',(#691,#361),#487,.F.);
#3567=ADVANCED_FACE('',(#692),#3366,.T.);
#3568=ADVANCED_FACE('',(#693,#362),#488,.T.);
#3569=ADVANCED_FACE('',(#694),#3367,.F.);
#3570=ADVANCED_FACE('',(#695),#3368,.T.);
#3571=ADVANCED_FACE('',(#696,#363),#489,.F.);
#3572=ADVANCED_FACE('',(#697,#364),#490,.F.);
#3573=ADVANCED_FACE('',(#698),#3369,.T.);
#3574=ADVANCED_FACE('',(#699,#365),#491,.T.);
#3575=ADVANCED_FACE('',(#700),#3370,.F.);
#3576=ADVANCED_FACE('',(#701),#3371,.T.);
#3577=ADVANCED_FACE('',(#702,#366),#492,.F.);
#3578=ADVANCED_FACE('',(#703),#3372,.F.);
#3579=ADVANCED_FACE('',(#704),#493,.T.);
#3580=ADVANCED_FACE('',(#705),#494,.T.);
#3581=ADVANCED_FACE('',(#706),#495,.T.);
#3582=ADVANCED_FACE('',(#707,#367),#496,.T.);
#3583=ADVANCED_FACE('',(#708,#368),#497,.F.);
#3584=ADVANCED_FACE('',(#709),#3373,.T.);
#3585=ADVANCED_FACE('',(#710),#3374,.T.);
#3586=ADVANCED_FACE('',(#711,#369),#498,.F.);
#3587=ADVANCED_FACE('',(#712),#3375,.T.);
#3588=ADVANCED_FACE('',(#713),#499,.T.);
#3589=ADVANCED_FACE('',(#714),#500,.F.);
#3590=CLOSED_SHELL('',(#3376,#3377,#3378,#3379,#3380,#3381,#3382,#3383,
#3384,#3385,#3386,#3387,#3388,#3389,#3390,#3391,#3392,#3393,#3394,#3395));
#3591=CLOSED_SHELL('',(#3396,#3397,#3398));
#3592=CLOSED_SHELL('',(#3399,#3400,#3401));
#3593=CLOSED_SHELL('',(#3402,#3403,#3404));
#3594=CLOSED_SHELL('',(#3405,#3406,#3407));
#3595=CLOSED_SHELL('',(#3408,#3409,#3410,#3411,#3412,#3413,#3414,#3415,
#3416,#3417,#3418,#3419,#3420,#3421,#3422,#3423,#3424,#3425,#3426,#3427,
#3428,#3429,#3430));
#3596=CLOSED_SHELL('',(#3431,#3432,#3433,#3434,#3435,#3436));
#3597=CLOSED_SHELL('',(#3437,#3438,#3439,#3440,#3441,#3442,#3443,#3444,
#3445,#3446,#3447,#3448,#3449));
#3598=CLOSED_SHELL('',(#3450,#3451,#3452,#3453,#3454,#3455,#3456,#3457,
#3458,#3459,#3460,#3461,#3462));
#3599=CLOSED_SHELL('',(#3463,#3464,#3465,#3466,#3467,#3468,#3469));
#3600=CLOSED_SHELL('',(#3470,#3471,#3472,#3473));
#3601=CLOSED_SHELL('',(#3474,#3475,#3476,#3477));
#3602=CLOSED_SHELL('',(#3478,#3479,#3480,#3481,#3482,#3483,#3484,#3485,
#3486,#3487,#3488,#3489,#3490));
#3603=CLOSED_SHELL('',(#3491,#3492,#3493,#3494));
#3604=CLOSED_SHELL('',(#3495,#3496,#3497,#3498));
#3605=CLOSED_SHELL('',(#3499,#3500,#3501,#3502,#3503,#3504,#3505,#3506));
#3606=CLOSED_SHELL('',(#3507,#3508,#3509,#3510,#3511,#3512,#3513,#3514));
#3607=CLOSED_SHELL('',(#3515,#3516,#3517,#3518,#3519,#3520,#3521,#3522));
#3608=CLOSED_SHELL('',(#3523,#3524,#3525,#3526,#3527,#3528,#3529,#3530));
#3609=CLOSED_SHELL('',(#3531,#3532,#3533,#3534,#3535,#3536,#3537,#3538,
#3539,#3540,#3541,#3542,#3543,#3544,#3545,#3546,#3547,#3548,#3549,#3550,
#3551,#3552,#3553));
#3610=CLOSED_SHELL('',(#3554,#3555,#3556,#3557,#3558,#3559));
#3611=CLOSED_SHELL('',(#3560,#3561,#3562,#3563,#3564,#3565));
#3612=CLOSED_SHELL('',(#3566,#3567,#3568,#3569,#3570,#3571));
#3613=CLOSED_SHELL('',(#3572,#3573,#3574,#3575,#3576,#3577));
#3614=CLOSED_SHELL('',(#3578,#3579,#3580,#3581,#3582,#3583,#3584,#3585,
#3586));
#3615=CLOSED_SHELL('',(#3587,#3588,#3589));
#3616=DERIVED_UNIT_ELEMENT(#3664,1.);
#3617=DERIVED_UNIT_ELEMENT(#6640,-3.);
#3618=DERIVED_UNIT_ELEMENT(#3664,1.);
#3619=DERIVED_UNIT_ELEMENT(#6640,-3.);
#3620=DERIVED_UNIT_ELEMENT(#3664,1.);
#3621=DERIVED_UNIT_ELEMENT(#6640,-3.);
#3622=DERIVED_UNIT_ELEMENT(#3664,1.);
#3623=DERIVED_UNIT_ELEMENT(#6640,-3.);
#3624=DERIVED_UNIT_ELEMENT(#3664,1.);
#3625=DERIVED_UNIT_ELEMENT(#6640,-3.);
#3626=DERIVED_UNIT_ELEMENT(#3664,1.);
#3627=DERIVED_UNIT_ELEMENT(#6640,-3.);
#3628=DERIVED_UNIT_ELEMENT(#3664,1.);
#3629=DERIVED_UNIT_ELEMENT(#6640,-3.);
#3630=DERIVED_UNIT_ELEMENT(#3664,1.);
#3631=DERIVED_UNIT_ELEMENT(#6640,-3.);
#3632=DERIVED_UNIT_ELEMENT(#3664,1.);
#3633=DERIVED_UNIT_ELEMENT(#6640,-3.);
#3634=DERIVED_UNIT_ELEMENT(#3664,1.);
#3635=DERIVED_UNIT_ELEMENT(#6640,-3.);
#3636=DERIVED_UNIT_ELEMENT(#3664,1.);
#3637=DERIVED_UNIT_ELEMENT(#6640,-3.);
#3638=DERIVED_UNIT_ELEMENT(#3664,1.);
#3639=DERIVED_UNIT_ELEMENT(#6640,-3.);
#3640=DERIVED_UNIT_ELEMENT(#3664,1.);
#3641=DERIVED_UNIT_ELEMENT(#6640,-3.);
#3642=DERIVED_UNIT_ELEMENT(#3664,1.);
#3643=DERIVED_UNIT_ELEMENT(#6640,-3.);
#3644=DERIVED_UNIT_ELEMENT(#3664,1.);
#3645=DERIVED_UNIT_ELEMENT(#6640,-3.);
#3646=DERIVED_UNIT_ELEMENT(#3664,1.);
#3647=DERIVED_UNIT_ELEMENT(#6640,-3.);
#3648=DERIVED_UNIT_ELEMENT(#3664,1.);
#3649=DERIVED_UNIT_ELEMENT(#6640,-3.);
#3650=DERIVED_UNIT_ELEMENT(#3664,1.);
#3651=DERIVED_UNIT_ELEMENT(#6640,-3.);
#3652=DERIVED_UNIT_ELEMENT(#3664,1.);
#3653=DERIVED_UNIT_ELEMENT(#6640,-3.);
#3654=DERIVED_UNIT_ELEMENT(#3664,1.);
#3655=DERIVED_UNIT_ELEMENT(#6640,-3.);
#3656=DERIVED_UNIT_ELEMENT(#3664,1.);
#3657=DERIVED_UNIT_ELEMENT(#6640,-3.);
#3658=DERIVED_UNIT_ELEMENT(#3664,1.);
#3659=DERIVED_UNIT_ELEMENT(#6640,-3.);
#3660=DERIVED_UNIT_ELEMENT(#3664,1.);
#3661=DERIVED_UNIT_ELEMENT(#6640,-3.);
#3662=DERIVED_UNIT_ELEMENT(#3664,1.);
#3663=DERIVED_UNIT_ELEMENT(#6640,-3.);
#3664=(
MASS_UNIT()
NAMED_UNIT(*)
SI_UNIT(.KILO.,.GRAM.)
);
#3665=DERIVED_UNIT((#3616,#3617));
#3666=DERIVED_UNIT((#3618,#3619));
#3667=DERIVED_UNIT((#3620,#3621));
#3668=DERIVED_UNIT((#3622,#3623));
#3669=DERIVED_UNIT((#3624,#3625));
#3670=DERIVED_UNIT((#3626,#3627));
#3671=DERIVED_UNIT((#3628,#3629));
#3672=DERIVED_UNIT((#3630,#3631));
#3673=DERIVED_UNIT((#3632,#3633));
#3674=DERIVED_UNIT((#3634,#3635));
#3675=DERIVED_UNIT((#3636,#3637));
#3676=DERIVED_UNIT((#3638,#3639));
#3677=DERIVED_UNIT((#3640,#3641));
#3678=DERIVED_UNIT((#3642,#3643));
#3679=DERIVED_UNIT((#3644,#3645));
#3680=DERIVED_UNIT((#3646,#3647));
#3681=DERIVED_UNIT((#3648,#3649));
#3682=DERIVED_UNIT((#3650,#3651));
#3683=DERIVED_UNIT((#3652,#3653));
#3684=DERIVED_UNIT((#3654,#3655));
#3685=DERIVED_UNIT((#3656,#3657));
#3686=DERIVED_UNIT((#3658,#3659));
#3687=DERIVED_UNIT((#3660,#3661));
#3688=DERIVED_UNIT((#3662,#3663));
#3689=MEASURE_REPRESENTATION_ITEM('density measure',
POSITIVE_RATIO_MEASURE(7850.),#3665);
#3690=MEASURE_REPRESENTATION_ITEM('density measure',
POSITIVE_RATIO_MEASURE(7850.),#3666);
#3691=MEASURE_REPRESENTATION_ITEM('density measure',
POSITIVE_RATIO_MEASURE(7850.),#3667);
#3692=MEASURE_REPRESENTATION_ITEM('density measure',
POSITIVE_RATIO_MEASURE(7850.),#3668);
#3693=MEASURE_REPRESENTATION_ITEM('density measure',
POSITIVE_RATIO_MEASURE(7850.),#3669);
#3694=MEASURE_REPRESENTATION_ITEM('density measure',
POSITIVE_RATIO_MEASURE(7850.),#3670);
#3695=MEASURE_REPRESENTATION_ITEM('density measure',
POSITIVE_RATIO_MEASURE(7850.),#3671);
#3696=MEASURE_REPRESENTATION_ITEM('density measure',
POSITIVE_RATIO_MEASURE(7850.),#3672);
#3697=MEASURE_REPRESENTATION_ITEM('density measure',
POSITIVE_RATIO_MEASURE(7850.),#3673);
#3698=MEASURE_REPRESENTATION_ITEM('density measure',
POSITIVE_RATIO_MEASURE(7850.),#3674);
#3699=MEASURE_REPRESENTATION_ITEM('density measure',
POSITIVE_RATIO_MEASURE(7850.),#3675);
#3700=MEASURE_REPRESENTATION_ITEM('density measure',
POSITIVE_RATIO_MEASURE(7850.),#3676);
#3701=MEASURE_REPRESENTATION_ITEM('density measure',
POSITIVE_RATIO_MEASURE(7850.),#3677);
#3702=MEASURE_REPRESENTATION_ITEM('density measure',
POSITIVE_RATIO_MEASURE(7850.),#3678);
#3703=MEASURE_REPRESENTATION_ITEM('density measure',
POSITIVE_RATIO_MEASURE(7850.),#3679);
#3704=MEASURE_REPRESENTATION_ITEM('density measure',
POSITIVE_RATIO_MEASURE(7850.),#3680);
#3705=MEASURE_REPRESENTATION_ITEM('density measure',
POSITIVE_RATIO_MEASURE(7850.),#3681);
#3706=MEASURE_REPRESENTATION_ITEM('density measure',
POSITIVE_RATIO_MEASURE(7850.),#3682);
#3707=MEASURE_REPRESENTATION_ITEM('density measure',
POSITIVE_RATIO_MEASURE(7850.),#3683);
#3708=MEASURE_REPRESENTATION_ITEM('density measure',
POSITIVE_RATIO_MEASURE(7850.),#3684);
#3709=MEASURE_REPRESENTATION_ITEM('density measure',
POSITIVE_RATIO_MEASURE(7850.),#3685);
#3710=MEASURE_REPRESENTATION_ITEM('density measure',
POSITIVE_RATIO_MEASURE(7850.),#3686);
#3711=MEASURE_REPRESENTATION_ITEM('density measure',
POSITIVE_RATIO_MEASURE(7850.),#3687);
#3712=MEASURE_REPRESENTATION_ITEM('density measure',
POSITIVE_RATIO_MEASURE(7850.),#3688);
#3713=PROPERTY_DEFINITION_REPRESENTATION(#3833,#3761);
#3714=PROPERTY_DEFINITION_REPRESENTATION(#3834,#3762);
#3715=PROPERTY_DEFINITION_REPRESENTATION(#3835,#3763);
#3716=PROPERTY_DEFINITION_REPRESENTATION(#3836,#3764);
#3717=PROPERTY_DEFINITION_REPRESENTATION(#3837,#3765);
#3718=PROPERTY_DEFINITION_REPRESENTATION(#3838,#3766);
#3719=PROPERTY_DEFINITION_REPRESENTATION(#3839,#3767);
#3720=PROPERTY_DEFINITION_REPRESENTATION(#3840,#3768);
#3721=PROPERTY_DEFINITION_REPRESENTATION(#3841,#3769);
#3722=PROPERTY_DEFINITION_REPRESENTATION(#3842,#3770);
#3723=PROPERTY_DEFINITION_REPRESENTATION(#3843,#3771);
#3724=PROPERTY_DEFINITION_REPRESENTATION(#3844,#3772);
#3725=PROPERTY_DEFINITION_REPRESENTATION(#3845,#3773);
#3726=PROPERTY_DEFINITION_REPRESENTATION(#3846,#3774);
#3727=PROPERTY_DEFINITION_REPRESENTATION(#3847,#3775);
#3728=PROPERTY_DEFINITION_REPRESENTATION(#3848,#3776);
#3729=PROPERTY_DEFINITION_REPRESENTATION(#3849,#3777);
#3730=PROPERTY_DEFINITION_REPRESENTATION(#3850,#3778);
#3731=PROPERTY_DEFINITION_REPRESENTATION(#3851,#3779);
#3732=PROPERTY_DEFINITION_REPRESENTATION(#3852,#3780);
#3733=PROPERTY_DEFINITION_REPRESENTATION(#3853,#3781);
#3734=PROPERTY_DEFINITION_REPRESENTATION(#3854,#3782);
#3735=PROPERTY_DEFINITION_REPRESENTATION(#3855,#3783);
#3736=PROPERTY_DEFINITION_REPRESENTATION(#3856,#3784);
#3737=PROPERTY_DEFINITION_REPRESENTATION(#3857,#3785);
#3738=PROPERTY_DEFINITION_REPRESENTATION(#3858,#3786);
#3739=PROPERTY_DEFINITION_REPRESENTATION(#3859,#3787);
#3740=PROPERTY_DEFINITION_REPRESENTATION(#3860,#3788);
#3741=PROPERTY_DEFINITION_REPRESENTATION(#3861,#3789);
#3742=PROPERTY_DEFINITION_REPRESENTATION(#3862,#3790);
#3743=PROPERTY_DEFINITION_REPRESENTATION(#3863,#3791);
#3744=PROPERTY_DEFINITION_REPRESENTATION(#3864,#3792);
#3745=PROPERTY_DEFINITION_REPRESENTATION(#3865,#3793);
#3746=PROPERTY_DEFINITION_REPRESENTATION(#3866,#3794);
#3747=PROPERTY_DEFINITION_REPRESENTATION(#3867,#3795);
#3748=PROPERTY_DEFINITION_REPRESENTATION(#3868,#3796);
#3749=PROPERTY_DEFINITION_REPRESENTATION(#3869,#3797);
#3750=PROPERTY_DEFINITION_REPRESENTATION(#3870,#3798);
#3751=PROPERTY_DEFINITION_REPRESENTATION(#3871,#3799);
#3752=PROPERTY_DEFINITION_REPRESENTATION(#3872,#3800);
#3753=PROPERTY_DEFINITION_REPRESENTATION(#3873,#3801);
#3754=PROPERTY_DEFINITION_REPRESENTATION(#3874,#3802);
#3755=PROPERTY_DEFINITION_REPRESENTATION(#3875,#3803);
#3756=PROPERTY_DEFINITION_REPRESENTATION(#3876,#3804);
#3757=PROPERTY_DEFINITION_REPRESENTATION(#3877,#3805);
#3758=PROPERTY_DEFINITION_REPRESENTATION(#3878,#3806);
#3759=PROPERTY_DEFINITION_REPRESENTATION(#3879,#3807);
#3760=PROPERTY_DEFINITION_REPRESENTATION(#3880,#3808);
#3761=REPRESENTATION('material name',(#3809),#6612);
#3762=REPRESENTATION('density',(#3689),#6612);
#3763=REPRESENTATION('material name',(#3810),#6613);
#3764=REPRESENTATION('density',(#3690),#6613);
#3765=REPRESENTATION('material name',(#3811),#6614);
#3766=REPRESENTATION('density',(#3691),#6614);
#3767=REPRESENTATION('material name',(#3812),#6615);
#3768=REPRESENTATION('density',(#3692),#6615);
#3769=REPRESENTATION('material name',(#3813),#6616);
#3770=REPRESENTATION('density',(#3693),#6616);
#3771=REPRESENTATION('material name',(#3814),#6617);
#3772=REPRESENTATION('density',(#3694),#6617);
#3773=REPRESENTATION('material name',(#3815),#6618);
#3774=REPRESENTATION('density',(#3695),#6618);
#3775=REPRESENTATION('material name',(#3816),#6619);
#3776=REPRESENTATION('density',(#3696),#6619);
#3777=REPRESENTATION('material name',(#3817),#6620);
#3778=REPRESENTATION('density',(#3697),#6620);
#3779=REPRESENTATION('material name',(#3818),#6621);
#3780=REPRESENTATION('density',(#3698),#6621);
#3781=REPRESENTATION('material name',(#3819),#6622);
#3782=REPRESENTATION('density',(#3699),#6622);
#3783=REPRESENTATION('material name',(#3820),#6623);
#3784=REPRESENTATION('density',(#3700),#6623);
#3785=REPRESENTATION('material name',(#3821),#6624);
#3786=REPRESENTATION('density',(#3701),#6624);
#3787=REPRESENTATION('material name',(#3822),#6625);
#3788=REPRESENTATION('density',(#3702),#6625);
#3789=REPRESENTATION('material name',(#3823),#6626);
#3790=REPRESENTATION('density',(#3703),#6626);
#3791=REPRESENTATION('material name',(#3824),#6627);
#3792=REPRESENTATION('density',(#3704),#6627);
#3793=REPRESENTATION('material name',(#3825),#6628);
#3794=REPRESENTATION('density',(#3705),#6628);
#3795=REPRESENTATION('material name',(#3826),#6630);
#3796=REPRESENTATION('density',(#3706),#6630);
#3797=REPRESENTATION('material name',(#3827),#6631);
#3798=REPRESENTATION('density',(#3707),#6631);
#3799=REPRESENTATION('material name',(#3828),#6632);
#3800=REPRESENTATION('density',(#3708),#6632);
#3801=REPRESENTATION('material name',(#3829),#6633);
#3802=REPRESENTATION('density',(#3709),#6633);
#3803=REPRESENTATION('material name',(#3830),#6634);
#3804=REPRESENTATION('density',(#3710),#6634);
#3805=REPRESENTATION('material name',(#3831),#6636);
#3806=REPRESENTATION('density',(#3711),#6636);
#3807=REPRESENTATION('material name',(#3832),#6637);
#3808=REPRESENTATION('density',(#3712),#6637);
#3809=DESCRIPTIVE_REPRESENTATION_ITEM('Steel','Steel');
#3810=DESCRIPTIVE_REPRESENTATION_ITEM('Steel','Steel');
#3811=DESCRIPTIVE_REPRESENTATION_ITEM('Steel','Steel');
#3812=DESCRIPTIVE_REPRESENTATION_ITEM('Steel','Steel');
#3813=DESCRIPTIVE_REPRESENTATION_ITEM('Steel','Steel');
#3814=DESCRIPTIVE_REPRESENTATION_ITEM('Steel','Steel');
#3815=DESCRIPTIVE_REPRESENTATION_ITEM('Steel','Steel');
#3816=DESCRIPTIVE_REPRESENTATION_ITEM('Steel','Steel');
#3817=DESCRIPTIVE_REPRESENTATION_ITEM('Steel','Steel');
#3818=DESCRIPTIVE_REPRESENTATION_ITEM('Steel','Steel');
#3819=DESCRIPTIVE_REPRESENTATION_ITEM('Steel','Steel');
#3820=DESCRIPTIVE_REPRESENTATION_ITEM('Steel','Steel');
#3821=DESCRIPTIVE_REPRESENTATION_ITEM('Steel','Steel');
#3822=DESCRIPTIVE_REPRESENTATION_ITEM('Steel','Steel');
#3823=DESCRIPTIVE_REPRESENTATION_ITEM('Steel','Steel');
#3824=DESCRIPTIVE_REPRESENTATION_ITEM('Steel','Steel');
#3825=DESCRIPTIVE_REPRESENTATION_ITEM('Steel','Steel');
#3826=DESCRIPTIVE_REPRESENTATION_ITEM('Steel','Steel');
#3827=DESCRIPTIVE_REPRESENTATION_ITEM('Steel','Steel');
#3828=DESCRIPTIVE_REPRESENTATION_ITEM('Steel','Steel');
#3829=DESCRIPTIVE_REPRESENTATION_ITEM('Steel','Steel');
#3830=DESCRIPTIVE_REPRESENTATION_ITEM('Steel','Steel');
#3831=DESCRIPTIVE_REPRESENTATION_ITEM('Steel','Steel');
#3832=DESCRIPTIVE_REPRESENTATION_ITEM('Steel','Steel');
#3833=PROPERTY_DEFINITION('material property','material name',#6768);
#3834=PROPERTY_DEFINITION('material property','density of part',#6768);
#3835=PROPERTY_DEFINITION('material property','material name',#6769);
#3836=PROPERTY_DEFINITION('material property','density of part',#6769);
#3837=PROPERTY_DEFINITION('material property','material name',#6770);
#3838=PROPERTY_DEFINITION('material property','density of part',#6770);
#3839=PROPERTY_DEFINITION('material property','material name',#6771);
#3840=PROPERTY_DEFINITION('material property','density of part',#6771);
#3841=PROPERTY_DEFINITION('material property','material name',#6772);
#3842=PROPERTY_DEFINITION('material property','density of part',#6772);
#3843=PROPERTY_DEFINITION('material property','material name',#6773);
#3844=PROPERTY_DEFINITION('material property','density of part',#6773);
#3845=PROPERTY_DEFINITION('material property','material name',#6774);
#3846=PROPERTY_DEFINITION('material property','density of part',#6774);
#3847=PROPERTY_DEFINITION('material property','material name',#6775);
#3848=PROPERTY_DEFINITION('material property','density of part',#6775);
#3849=PROPERTY_DEFINITION('material property','material name',#6776);
#3850=PROPERTY_DEFINITION('material property','density of part',#6776);
#3851=PROPERTY_DEFINITION('material property','material name',#6777);
#3852=PROPERTY_DEFINITION('material property','density of part',#6777);
#3853=PROPERTY_DEFINITION('material property','material name',#6778);
#3854=PROPERTY_DEFINITION('material property','density of part',#6778);
#3855=PROPERTY_DEFINITION('material property','material name',#6779);
#3856=PROPERTY_DEFINITION('material property','density of part',#6779);
#3857=PROPERTY_DEFINITION('material property','material name',#6780);
#3858=PROPERTY_DEFINITION('material property','density of part',#6780);
#3859=PROPERTY_DEFINITION('material property','material name',#6781);
#3860=PROPERTY_DEFINITION('material property','density of part',#6781);
#3861=PROPERTY_DEFINITION('material property','material name',#6782);
#3862=PROPERTY_DEFINITION('material property','density of part',#6782);
#3863=PROPERTY_DEFINITION('material property','material name',#6783);
#3864=PROPERTY_DEFINITION('material property','density of part',#6783);
#3865=PROPERTY_DEFINITION('material property','material name',#6784);
#3866=PROPERTY_DEFINITION('material property','density of part',#6784);
#3867=PROPERTY_DEFINITION('material property','material name',#6786);
#3868=PROPERTY_DEFINITION('material property','density of part',#6786);
#3869=PROPERTY_DEFINITION('material property','material name',#6787);
#3870=PROPERTY_DEFINITION('material property','density of part',#6787);
#3871=PROPERTY_DEFINITION('material property','material name',#6788);
#3872=PROPERTY_DEFINITION('material property','density of part',#6788);
#3873=PROPERTY_DEFINITION('material property','material name',#6789);
#3874=PROPERTY_DEFINITION('material property','density of part',#6789);
#3875=PROPERTY_DEFINITION('material property','material name',#6790);
#3876=PROPERTY_DEFINITION('material property','density of part',#6790);
#3877=PROPERTY_DEFINITION('material property','material name',#6792);
#3878=PROPERTY_DEFINITION('material property','density of part',#6792);
#3879=PROPERTY_DEFINITION('material property','material name',#6793);
#3880=PROPERTY_DEFINITION('material property','density of part',#6793);
#3881=AXIS2_PLACEMENT_3D('',#5486,#4329,#4330);
#3882=AXIS2_PLACEMENT_3D('',#5487,#4331,#4332);
#3883=AXIS2_PLACEMENT_3D('',#5488,#4333,#4334);
#3884=AXIS2_PLACEMENT_3D('',#5489,#4335,#4336);
#3885=AXIS2_PLACEMENT_3D('',#5491,#4337,#4338);
#3886=AXIS2_PLACEMENT_3D('',#5494,#4340,#4341);
#3887=AXIS2_PLACEMENT_3D('',#5495,#4342,#4343);
#3888=AXIS2_PLACEMENT_3D('',#5497,#4344,#4345);
#3889=AXIS2_PLACEMENT_3D('',#5500,#4347,#4348);
#3890=AXIS2_PLACEMENT_3D('',#5501,#4349,#4350);
#3891=AXIS2_PLACEMENT_3D('',#5503,#4351,#4352);
#3892=AXIS2_PLACEMENT_3D('',#5506,#4354,#4355);
#3893=AXIS2_PLACEMENT_3D('',#5507,#4356,#4357);
#3894=AXIS2_PLACEMENT_3D('',#5509,#4358,#4359);
#3895=AXIS2_PLACEMENT_3D('',#5512,#4361,#4362);
#3896=AXIS2_PLACEMENT_3D('',#5513,#4363,#4364);
#3897=AXIS2_PLACEMENT_3D('',#5515,#4365,#4366);
#3898=AXIS2_PLACEMENT_3D('',#5518,#4368,#4369);
#3899=AXIS2_PLACEMENT_3D('',#5519,#4370,#4371);
#3900=AXIS2_PLACEMENT_3D('',#5521,#4372,#4373);
#3901=AXIS2_PLACEMENT_3D('',#5524,#4375,#4376);
#3902=AXIS2_PLACEMENT_3D('',#5525,#4377,#4378);
#3903=AXIS2_PLACEMENT_3D('',#5527,#4379,#4380);
#3904=AXIS2_PLACEMENT_3D('',#5530,#4382,#4383);
#3905=AXIS2_PLACEMENT_3D('',#5531,#4384,#4385);
#3906=AXIS2_PLACEMENT_3D('',#5533,#4386,#4387);
#3907=AXIS2_PLACEMENT_3D('',#5536,#4389,#4390);
#3908=AXIS2_PLACEMENT_3D('',#5537,#4391,#4392);
#3909=AXIS2_PLACEMENT_3D('',#5539,#4393,#4394);
#3910=AXIS2_PLACEMENT_3D('',#5542,#4396,#4397);
#3911=AXIS2_PLACEMENT_3D('',#5543,#4398,#4399);
#3912=AXIS2_PLACEMENT_3D('',#5545,#4400,#4401);
#3913=AXIS2_PLACEMENT_3D('',#5548,#4403,#4404);
#3914=AXIS2_PLACEMENT_3D('',#5549,#4405,#4406);
#3915=AXIS2_PLACEMENT_3D('',#5551,#4407,#4408);
#3916=AXIS2_PLACEMENT_3D('',#5554,#4410,#4411);
#3917=AXIS2_PLACEMENT_3D('',#5555,#4412,#4413);
#3918=AXIS2_PLACEMENT_3D('',#5557,#4414,#4415);
#3919=AXIS2_PLACEMENT_3D('',#5560,#4417,#4418);
#3920=AXIS2_PLACEMENT_3D('',#5561,#4419,#4420);
#3921=AXIS2_PLACEMENT_3D('',#5563,#4421,#4422);
#3922=AXIS2_PLACEMENT_3D('',#5566,#4424,#4425);
#3923=AXIS2_PLACEMENT_3D('',#5567,#4426,#4427);
#3924=AXIS2_PLACEMENT_3D('',#5569,#4428,#4429);
#3925=AXIS2_PLACEMENT_3D('',#5572,#4431,#4432);
#3926=AXIS2_PLACEMENT_3D('',#5573,#4433,#4434);
#3927=AXIS2_PLACEMENT_3D('',#5582,#4439,#4440);
#3928=AXIS2_PLACEMENT_3D('',#5588,#4444,#4445);
#3929=AXIS2_PLACEMENT_3D('',#5594,#4449,#4450);
#3930=AXIS2_PLACEMENT_3D('',#5597,#4453,#4454);
#3931=AXIS2_PLACEMENT_3D('',#5598,#4455,#4456);
#3932=AXIS2_PLACEMENT_3D('',#5599,#4457,#4458);
#3933=AXIS2_PLACEMENT_3D('',#5600,#4459,#4460);
#3934=AXIS2_PLACEMENT_3D('',#5602,#4461,#4462);
#3935=AXIS2_PLACEMENT_3D('',#5605,#4464,#4465);
#3936=AXIS2_PLACEMENT_3D('',#5606,#4466,#4467);
#3937=AXIS2_PLACEMENT_3D('',#5607,#4468,#4469);
#3938=AXIS2_PLACEMENT_3D('',#5608,#4470,#4471);
#3939=AXIS2_PLACEMENT_3D('',#5609,#4472,#4473);
#3940=AXIS2_PLACEMENT_3D('',#5611,#4474,#4475);
#3941=AXIS2_PLACEMENT_3D('',#5614,#4477,#4478);
#3942=AXIS2_PLACEMENT_3D('',#5615,#4479,#4480);
#3943=AXIS2_PLACEMENT_3D('',#5616,#4481,#4482);
#3944=AXIS2_PLACEMENT_3D('',#5617,#4483,#4484);
#3945=AXIS2_PLACEMENT_3D('',#5618,#4485,#4486);
#3946=AXIS2_PLACEMENT_3D('',#5620,#4487,#4488);
#3947=AXIS2_PLACEMENT_3D('',#5623,#4490,#4491);
#3948=AXIS2_PLACEMENT_3D('',#5624,#4492,#4493);
#3949=AXIS2_PLACEMENT_3D('',#5625,#4494,#4495);
#3950=AXIS2_PLACEMENT_3D('',#5626,#4496,#4497);
#3951=AXIS2_PLACEMENT_3D('',#5627,#4498,#4499);
#3952=AXIS2_PLACEMENT_3D('',#5629,#4500,#4501);
#3953=AXIS2_PLACEMENT_3D('',#5632,#4503,#4504);
#3954=AXIS2_PLACEMENT_3D('',#5633,#4505,#4506);
#3955=AXIS2_PLACEMENT_3D('',#5634,#4507,#4508);
#3956=AXIS2_PLACEMENT_3D('',#5635,#4509,#4510);
#3957=AXIS2_PLACEMENT_3D('',#5636,#4511,#4512);
#3958=AXIS2_PLACEMENT_3D('',#5638,#4513,#4514);
#3959=AXIS2_PLACEMENT_3D('',#5641,#4516,#4517);
#3960=AXIS2_PLACEMENT_3D('',#5642,#4518,#4519);
#3961=AXIS2_PLACEMENT_3D('',#5644,#4520,#4521);
#3962=AXIS2_PLACEMENT_3D('',#5645,#4522,#4523);
#3963=AXIS2_PLACEMENT_3D('',#5647,#4524,#4525);
#3964=AXIS2_PLACEMENT_3D('',#5650,#4527,#4528);
#3965=AXIS2_PLACEMENT_3D('',#5651,#4529,#4530);
#3966=AXIS2_PLACEMENT_3D('',#5653,#4531,#4532);
#3967=AXIS2_PLACEMENT_3D('',#5654,#4533,#4534);
#3968=AXIS2_PLACEMENT_3D('',#5656,#4535,#4536);
#3969=AXIS2_PLACEMENT_3D('',#5659,#4538,#4539);
#3970=AXIS2_PLACEMENT_3D('',#5660,#4540,#4541);
#3971=AXIS2_PLACEMENT_3D('',#5662,#4542,#4543);
#3972=AXIS2_PLACEMENT_3D('',#5663,#4544,#4545);
#3973=AXIS2_PLACEMENT_3D('',#5665,#4546,#4547);
#3974=AXIS2_PLACEMENT_3D('',#5668,#4549,#4550);
#3975=AXIS2_PLACEMENT_3D('',#5669,#4551,#4552);
#3976=AXIS2_PLACEMENT_3D('',#5671,#4553,#4554);
#3977=AXIS2_PLACEMENT_3D('',#5672,#4555,#4556);
#3978=AXIS2_PLACEMENT_3D('',#5674,#4557,#4558);
#3979=AXIS2_PLACEMENT_3D('',#5676,#4560,#4561);
#3980=AXIS2_PLACEMENT_3D('',#5678,#4562,#4563);
#3981=AXIS2_PLACEMENT_3D('',#5680,#4565,#4566);
#3982=AXIS2_PLACEMENT_3D('',#5682,#4567,#4568);
#3983=AXIS2_PLACEMENT_3D('',#5684,#4570,#4571);
#3984=AXIS2_PLACEMENT_3D('',#5686,#4572,#4573);
#3985=AXIS2_PLACEMENT_3D('',#5688,#4575,#4576);
#3986=AXIS2_PLACEMENT_3D('',#5697,#4581,#4582);
#3987=AXIS2_PLACEMENT_3D('',#5703,#4586,#4587);
#3988=AXIS2_PLACEMENT_3D('',#5709,#4591,#4592);
#3989=AXIS2_PLACEMENT_3D('',#5712,#4595,#4596);
#3990=AXIS2_PLACEMENT_3D('',#5713,#4597,#4598);
#3991=AXIS2_PLACEMENT_3D('',#5722,#4603,#4604);
#3992=AXIS2_PLACEMENT_3D('',#5728,#4608,#4609);
#3993=AXIS2_PLACEMENT_3D('',#5734,#4613,#4614);
#3994=AXIS2_PLACEMENT_3D('',#5737,#4617,#4618);
#3995=AXIS2_PLACEMENT_3D('',#5738,#4619,#4620);
#3996=AXIS2_PLACEMENT_3D('',#5739,#4621,#4622);
#3997=AXIS2_PLACEMENT_3D('',#5740,#4623,#4624);
#3998=AXIS2_PLACEMENT_3D('',#5749,#4629,#4630);
#3999=AXIS2_PLACEMENT_3D('',#5755,#4634,#4635);
#4000=AXIS2_PLACEMENT_3D('',#5761,#4639,#4640);
#4001=AXIS2_PLACEMENT_3D('',#5764,#4643,#4644);
#4002=AXIS2_PLACEMENT_3D('',#5765,#4645,#4646);
#4003=AXIS2_PLACEMENT_3D('',#5766,#4647,#4648);
#4004=AXIS2_PLACEMENT_3D('',#5767,#4649,#4650);
#4005=AXIS2_PLACEMENT_3D('',#5769,#4651,#4652);
#4006=AXIS2_PLACEMENT_3D('',#5772,#4654,#4655);
#4007=AXIS2_PLACEMENT_3D('',#5824,#4656,#4657);
#4008=AXIS2_PLACEMENT_3D('',#5826,#4658,#4659);
#4009=AXIS2_PLACEMENT_3D('',#5827,#4660,#4661);
#4010=AXIS2_PLACEMENT_3D('',#5829,#4662,#4663);
#4011=AXIS2_PLACEMENT_3D('',#5831,#4665,#4666);
#4012=AXIS2_PLACEMENT_3D('',#5833,#4667,#4668);
#4013=AXIS2_PLACEMENT_3D('',#5836,#4670,#4671);
#4014=AXIS2_PLACEMENT_3D('',#5837,#4672,#4673);
#4015=AXIS2_PLACEMENT_3D('',#5839,#4674,#4675);
#4016=AXIS2_PLACEMENT_3D('',#5842,#4677,#4678);
#4017=AXIS2_PLACEMENT_3D('',#5843,#4679,#4680);
#4018=AXIS2_PLACEMENT_3D('',#5852,#4685,#4686);
#4019=AXIS2_PLACEMENT_3D('',#5858,#4690,#4691);
#4020=AXIS2_PLACEMENT_3D('',#5864,#4695,#4696);
#4021=AXIS2_PLACEMENT_3D('',#5870,#4700,#4701);
#4022=AXIS2_PLACEMENT_3D('',#5876,#4705,#4706);
#4023=AXIS2_PLACEMENT_3D('',#5879,#4709,#4710);
#4024=AXIS2_PLACEMENT_3D('',#5880,#4711,#4712);
#4025=AXIS2_PLACEMENT_3D('',#5881,#4713,#4714);
#4026=AXIS2_PLACEMENT_3D('',#5882,#4715,#4716);
#4027=AXIS2_PLACEMENT_3D('',#5884,#4717,#4718);
#4028=AXIS2_PLACEMENT_3D('',#5887,#4720,#4721);
#4029=AXIS2_PLACEMENT_3D('',#5939,#4722,#4723);
#4030=AXIS2_PLACEMENT_3D('',#5941,#4724,#4725);
#4031=AXIS2_PLACEMENT_3D('',#5942,#4726,#4727);
#4032=AXIS2_PLACEMENT_3D('',#5944,#4728,#4729);
#4033=AXIS2_PLACEMENT_3D('',#5946,#4731,#4732);
#4034=AXIS2_PLACEMENT_3D('',#5948,#4733,#4734);
#4035=AXIS2_PLACEMENT_3D('',#5951,#4736,#4737);
#4036=AXIS2_PLACEMENT_3D('',#5952,#4738,#4739);
#4037=AXIS2_PLACEMENT_3D('',#5954,#4740,#4741);
#4038=AXIS2_PLACEMENT_3D('',#5957,#4743,#4744);
#4039=AXIS2_PLACEMENT_3D('',#5958,#4745,#4746);
#4040=AXIS2_PLACEMENT_3D('',#5967,#4751,#4752);
#4041=AXIS2_PLACEMENT_3D('',#5973,#4756,#4757);
#4042=AXIS2_PLACEMENT_3D('',#5979,#4761,#4762);
#4043=AXIS2_PLACEMENT_3D('',#5985,#4766,#4767);
#4044=AXIS2_PLACEMENT_3D('',#5991,#4771,#4772);
#4045=AXIS2_PLACEMENT_3D('',#5994,#4775,#4776);
#4046=AXIS2_PLACEMENT_3D('',#5995,#4777,#4778);
#4047=AXIS2_PLACEMENT_3D('',#5996,#4779,#4780);
#4048=AXIS2_PLACEMENT_3D('',#5997,#4781,#4782);
#4049=AXIS2_PLACEMENT_3D('',#5999,#4783,#4784);
#4050=AXIS2_PLACEMENT_3D('',#6002,#4786,#4787);
#4051=AXIS2_PLACEMENT_3D('',#6003,#4788,#4789);
#4052=AXIS2_PLACEMENT_3D('',#6004,#4790,#4791);
#4053=AXIS2_PLACEMENT_3D('',#6006,#4792,#4793);
#4054=AXIS2_PLACEMENT_3D('',#6009,#4795,#4796);
#4055=AXIS2_PLACEMENT_3D('',#6010,#4797,#4798);
#4056=AXIS2_PLACEMENT_3D('',#6011,#4799,#4800);
#4057=AXIS2_PLACEMENT_3D('',#6013,#4801,#4802);
#4058=AXIS2_PLACEMENT_3D('',#6016,#4804,#4805);
#4059=AXIS2_PLACEMENT_3D('',#6017,#4806,#4807);
#4060=AXIS2_PLACEMENT_3D('',#6018,#4808,#4809);
#4061=AXIS2_PLACEMENT_3D('',#6019,#4810,#4811);
#4062=AXIS2_PLACEMENT_3D('',#6020,#4812,#4813);
#4063=AXIS2_PLACEMENT_3D('',#6022,#4814,#4815);
#4064=AXIS2_PLACEMENT_3D('',#6025,#4817,#4818);
#4065=AXIS2_PLACEMENT_3D('',#6026,#4819,#4820);
#4066=AXIS2_PLACEMENT_3D('',#6028,#4821,#4822);
#4067=AXIS2_PLACEMENT_3D('',#6031,#4824,#4825);
#4068=AXIS2_PLACEMENT_3D('',#6032,#4826,#4827);
#4069=AXIS2_PLACEMENT_3D('',#6033,#4828,#4829);
#4070=AXIS2_PLACEMENT_3D('',#6034,#4830,#4831);
#4071=AXIS2_PLACEMENT_3D('',#6035,#4832,#4833);
#4072=AXIS2_PLACEMENT_3D('',#6037,#4834,#4835);
#4073=AXIS2_PLACEMENT_3D('',#6040,#4837,#4838);
#4074=AXIS2_PLACEMENT_3D('',#6041,#4839,#4840);
#4075=AXIS2_PLACEMENT_3D('',#6043,#4841,#4842);
#4076=AXIS2_PLACEMENT_3D('',#6046,#4844,#4845);
#4077=AXIS2_PLACEMENT_3D('',#6047,#4846,#4847);
#4078=AXIS2_PLACEMENT_3D('',#6048,#4848,#4849);
#4079=AXIS2_PLACEMENT_3D('',#6049,#4850,#4851);
#4080=AXIS2_PLACEMENT_3D('',#6050,#4852,#4853);
#4081=AXIS2_PLACEMENT_3D('',#6052,#4854,#4855);
#4082=AXIS2_PLACEMENT_3D('',#6055,#4857,#4858);
#4083=AXIS2_PLACEMENT_3D('',#6056,#4859,#4860);
#4084=AXIS2_PLACEMENT_3D('',#6057,#4861,#4862);
#4085=AXIS2_PLACEMENT_3D('',#6060,#4863,#4864);
#4086=AXIS2_PLACEMENT_3D('',#6061,#4865,#4866);
#4087=AXIS2_PLACEMENT_3D('',#6062,#4867,#4868);
#4088=AXIS2_PLACEMENT_3D('',#6064,#4869,#4870);
#4089=AXIS2_PLACEMENT_3D('',#6068,#4872,#4873);
#4090=AXIS2_PLACEMENT_3D('',#6072,#4876,#4877);
#4091=AXIS2_PLACEMENT_3D('',#6073,#4878,#4879);
#4092=AXIS2_PLACEMENT_3D('',#6076,#4880,#4881);
#4093=AXIS2_PLACEMENT_3D('',#6077,#4882,#4883);
#4094=AXIS2_PLACEMENT_3D('',#6078,#4884,#4885);
#4095=AXIS2_PLACEMENT_3D('',#6080,#4886,#4887);
#4096=AXIS2_PLACEMENT_3D('',#6084,#4889,#4890);
#4097=AXIS2_PLACEMENT_3D('',#6088,#4893,#4894);
#4098=AXIS2_PLACEMENT_3D('',#6089,#4895,#4896);
#4099=AXIS2_PLACEMENT_3D('',#6091,#4897,#4898);
#4100=AXIS2_PLACEMENT_3D('',#6094,#4900,#4901);
#4101=AXIS2_PLACEMENT_3D('',#6095,#4902,#4903);
#4102=AXIS2_PLACEMENT_3D('',#6096,#4904,#4905);
#4103=AXIS2_PLACEMENT_3D('',#6097,#4906,#4907);
#4104=AXIS2_PLACEMENT_3D('',#6099,#4908,#4909);
#4105=AXIS2_PLACEMENT_3D('',#6100,#4910,#4911);
#4106=AXIS2_PLACEMENT_3D('',#6103,#4913,#4914);
#4107=AXIS2_PLACEMENT_3D('',#6104,#4915,#4916);
#4108=AXIS2_PLACEMENT_3D('',#6106,#4917,#4918);
#4109=AXIS2_PLACEMENT_3D('',#6109,#4920,#4921);
#4110=AXIS2_PLACEMENT_3D('',#6110,#4922,#4923);
#4111=AXIS2_PLACEMENT_3D('',#6111,#4924,#4925);
#4112=AXIS2_PLACEMENT_3D('',#6112,#4926,#4927);
#4113=AXIS2_PLACEMENT_3D('',#6113,#4928,#4929);
#4114=AXIS2_PLACEMENT_3D('',#6114,#4930,#4931);
#4115=AXIS2_PLACEMENT_3D('',#6116,#4932,#4933);
#4116=AXIS2_PLACEMENT_3D('',#6119,#4935,#4936);
#4117=AXIS2_PLACEMENT_3D('',#6120,#4937,#4938);
#4118=AXIS2_PLACEMENT_3D('',#6122,#4939,#4940);
#4119=AXIS2_PLACEMENT_3D('',#6125,#4942,#4943);
#4120=AXIS2_PLACEMENT_3D('',#6126,#4944,#4945);
#4121=AXIS2_PLACEMENT_3D('',#6127,#4946,#4947);
#4122=AXIS2_PLACEMENT_3D('',#6128,#4948,#4949);
#4123=AXIS2_PLACEMENT_3D('',#6129,#4950,#4951);
#4124=AXIS2_PLACEMENT_3D('',#6131,#4952,#4953);
#4125=AXIS2_PLACEMENT_3D('',#6134,#4955,#4956);
#4126=AXIS2_PLACEMENT_3D('',#6135,#4957,#4958);
#4127=AXIS2_PLACEMENT_3D('',#6137,#4959,#4960);
#4128=AXIS2_PLACEMENT_3D('',#6140,#4962,#4963);
#4129=AXIS2_PLACEMENT_3D('',#6141,#4964,#4965);
#4130=AXIS2_PLACEMENT_3D('',#6142,#4966,#4967);
#4131=AXIS2_PLACEMENT_3D('',#6143,#4968,#4969);
#4132=AXIS2_PLACEMENT_3D('',#6144,#4970,#4971);
#4133=AXIS2_PLACEMENT_3D('',#6153,#4976,#4977);
#4134=AXIS2_PLACEMENT_3D('',#6159,#4981,#4982);
#4135=AXIS2_PLACEMENT_3D('',#6165,#4986,#4987);
#4136=AXIS2_PLACEMENT_3D('',#6171,#4991,#4992);
#4137=AXIS2_PLACEMENT_3D('',#6177,#4996,#4997);
#4138=AXIS2_PLACEMENT_3D('',#6180,#5000,#5001);
#4139=AXIS2_PLACEMENT_3D('',#6181,#5002,#5003);
#4140=AXIS2_PLACEMENT_3D('',#6182,#5004,#5005);
#4141=AXIS2_PLACEMENT_3D('',#6184,#5006,#5007);
#4142=AXIS2_PLACEMENT_3D('',#6185,#5008,#5009);
#4143=AXIS2_PLACEMENT_3D('',#6187,#5010,#5011);
#4144=AXIS2_PLACEMENT_3D('',#6188,#5012,#5013);
#4145=AXIS2_PLACEMENT_3D('',#6190,#5014,#5015);
#4146=AXIS2_PLACEMENT_3D('',#6192,#5017,#5018);
#4147=AXIS2_PLACEMENT_3D('',#6194,#5019,#5020);
#4148=AXIS2_PLACEMENT_3D('',#6196,#5022,#5023);
#4149=AXIS2_PLACEMENT_3D('',#6198,#5024,#5025);
#4150=AXIS2_PLACEMENT_3D('',#6200,#5027,#5028);
#4151=AXIS2_PLACEMENT_3D('',#6202,#5029,#5030);
#4152=AXIS2_PLACEMENT_3D('',#6203,#5031,#5032);
#4153=AXIS2_PLACEMENT_3D('',#6205,#5033,#5034);
#4154=AXIS2_PLACEMENT_3D('',#6207,#5036,#5037);
#4155=AXIS2_PLACEMENT_3D('',#6209,#5039,#5040);
#4156=AXIS2_PLACEMENT_3D('',#6210,#5041,#5042);
#4157=AXIS2_PLACEMENT_3D('',#6219,#5047,#5048);
#4158=AXIS2_PLACEMENT_3D('',#6225,#5052,#5053);
#4159=AXIS2_PLACEMENT_3D('',#6231,#5057,#5058);
#4160=AXIS2_PLACEMENT_3D('',#6237,#5062,#5063);
#4161=AXIS2_PLACEMENT_3D('',#6243,#5067,#5068);
#4162=AXIS2_PLACEMENT_3D('',#6246,#5071,#5072);
#4163=AXIS2_PLACEMENT_3D('',#6247,#5073,#5074);
#4164=AXIS2_PLACEMENT_3D('',#6248,#5075,#5076);
#4165=AXIS2_PLACEMENT_3D('',#6250,#5077,#5078);
#4166=AXIS2_PLACEMENT_3D('',#6251,#5079,#5080);
#4167=AXIS2_PLACEMENT_3D('',#6253,#5081,#5082);
#4168=AXIS2_PLACEMENT_3D('',#6254,#5083,#5084);
#4169=AXIS2_PLACEMENT_3D('',#6256,#5085,#5086);
#4170=AXIS2_PLACEMENT_3D('',#6258,#5088,#5089);
#4171=AXIS2_PLACEMENT_3D('',#6260,#5090,#5091);
#4172=AXIS2_PLACEMENT_3D('',#6262,#5093,#5094);
#4173=AXIS2_PLACEMENT_3D('',#6264,#5095,#5096);
#4174=AXIS2_PLACEMENT_3D('',#6266,#5098,#5099);
#4175=AXIS2_PLACEMENT_3D('',#6268,#5100,#5101);
#4176=AXIS2_PLACEMENT_3D('',#6269,#5102,#5103);
#4177=AXIS2_PLACEMENT_3D('',#6271,#5104,#5105);
#4178=AXIS2_PLACEMENT_3D('',#6273,#5107,#5108);
#4179=AXIS2_PLACEMENT_3D('',#6275,#5110,#5111);
#4180=AXIS2_PLACEMENT_3D('',#6276,#5112,#5113);
#4181=AXIS2_PLACEMENT_3D('',#6277,#5114,#5115);
#4182=AXIS2_PLACEMENT_3D('',#6278,#5116,#5117);
#4183=AXIS2_PLACEMENT_3D('',#6279,#5118,#5119);
#4184=AXIS2_PLACEMENT_3D('',#6280,#5120,#5121);
#4185=AXIS2_PLACEMENT_3D('',#6281,#5122,#5123);
#4186=AXIS2_PLACEMENT_3D('',#6282,#5124,#5125);
#4187=AXIS2_PLACEMENT_3D('',#6283,#5126,#5127);
#4188=AXIS2_PLACEMENT_3D('',#6284,#5128,#5129);
#4189=AXIS2_PLACEMENT_3D('',#6285,#5130,#5131);
#4190=AXIS2_PLACEMENT_3D('',#6286,#5132,#5133);
#4191=AXIS2_PLACEMENT_3D('',#6287,#5134,#5135);
#4192=AXIS2_PLACEMENT_3D('',#6288,#5136,#5137);
#4193=AXIS2_PLACEMENT_3D('',#6289,#5138,#5139);
#4194=AXIS2_PLACEMENT_3D('',#6290,#5140,#5141);
#4195=AXIS2_PLACEMENT_3D('',#6291,#5142,#5143);
#4196=AXIS2_PLACEMENT_3D('',#6292,#5144,#5145);
#4197=AXIS2_PLACEMENT_3D('',#6293,#5146,#5147);
#4198=AXIS2_PLACEMENT_3D('',#6294,#5148,#5149);
#4199=AXIS2_PLACEMENT_3D('',#6295,#5150,#5151);
#4200=AXIS2_PLACEMENT_3D('',#6296,#5152,#5153);
#4201=AXIS2_PLACEMENT_3D('',#6297,#5154,#5155);
#4202=AXIS2_PLACEMENT_3D('',#6298,#5156,#5157);
#4203=AXIS2_PLACEMENT_3D('',#6299,#5158,#5159);
#4204=AXIS2_PLACEMENT_3D('',#6300,#5160,#5161);
#4205=AXIS2_PLACEMENT_3D('',#6301,#5162,#5163);
#4206=AXIS2_PLACEMENT_3D('',#6302,#5164,#5165);
#4207=AXIS2_PLACEMENT_3D('',#6303,#5166,#5167);
#4208=AXIS2_PLACEMENT_3D('',#6304,#5168,#5169);
#4209=AXIS2_PLACEMENT_3D('',#6305,#5170,#5171);
#4210=AXIS2_PLACEMENT_3D('',#6307,#5172,#5173);
#4211=AXIS2_PLACEMENT_3D('',#6310,#5175,#5176);
#4212=AXIS2_PLACEMENT_3D('',#6311,#5177,#5178);
#4213=AXIS2_PLACEMENT_3D('',#6313,#5179,#5180);
#4214=AXIS2_PLACEMENT_3D('',#6316,#5182,#5183);
#4215=AXIS2_PLACEMENT_3D('',#6317,#5184,#5185);
#4216=AXIS2_PLACEMENT_3D('',#6319,#5186,#5187);
#4217=AXIS2_PLACEMENT_3D('',#6322,#5189,#5190);
#4218=AXIS2_PLACEMENT_3D('',#6323,#5191,#5192);
#4219=AXIS2_PLACEMENT_3D('',#6325,#5193,#5194);
#4220=AXIS2_PLACEMENT_3D('',#6328,#5196,#5197);
#4221=AXIS2_PLACEMENT_3D('',#6329,#5198,#5199);
#4222=AXIS2_PLACEMENT_3D('',#6332,#5200,#5201);
#4223=AXIS2_PLACEMENT_3D('',#6339,#5205,#5206);
#4224=AXIS2_PLACEMENT_3D('',#6340,#5207,#5208);
#4225=AXIS2_PLACEMENT_3D('',#6346,#5212,#5213);
#4226=AXIS2_PLACEMENT_3D('',#6348,#5214,#5215);
#4227=AXIS2_PLACEMENT_3D('',#6353,#5218,#5219);
#4228=AXIS2_PLACEMENT_3D('',#6354,#5220,#5221);
#4229=AXIS2_PLACEMENT_3D('',#6356,#5223,#5224);
#4230=AXIS2_PLACEMENT_3D('',#6358,#5226,#5227);
#4231=AXIS2_PLACEMENT_3D('',#6368,#5233,#5234);
#4232=AXIS2_PLACEMENT_3D('',#6374,#5238,#5239);
#4233=AXIS2_PLACEMENT_3D('',#6380,#5243,#5244);
#4234=AXIS2_PLACEMENT_3D('',#6386,#5248,#5249);
#4235=AXIS2_PLACEMENT_3D('',#6402,#5258,#5259);
#4236=AXIS2_PLACEMENT_3D('',#6406,#5262,#5263);
#4237=AXIS2_PLACEMENT_3D('',#6410,#5266,#5267);
#4238=AXIS2_PLACEMENT_3D('',#6414,#5270,#5271);
#4239=AXIS2_PLACEMENT_3D('',#6418,#5274,#5275);
#4240=AXIS2_PLACEMENT_3D('',#6422,#5278,#5279);
#4241=AXIS2_PLACEMENT_3D('',#6428,#5283,#5284);
#4242=AXIS2_PLACEMENT_3D('',#6430,#5286,#5287);
#4243=AXIS2_PLACEMENT_3D('',#6432,#5289,#5290);
#4244=AXIS2_PLACEMENT_3D('',#6433,#5291,#5292);
#4245=AXIS2_PLACEMENT_3D('',#6434,#5293,#5294);
#4246=AXIS2_PLACEMENT_3D('',#6436,#5295,#5296);
#4247=AXIS2_PLACEMENT_3D('',#6438,#5297,#5298);
#4248=AXIS2_PLACEMENT_3D('',#6439,#5299,#5300);
#4249=AXIS2_PLACEMENT_3D('',#6441,#5301,#5302);
#4250=AXIS2_PLACEMENT_3D('',#6443,#5304,#5305);
#4251=AXIS2_PLACEMENT_3D('',#6445,#5306,#5307);
#4252=AXIS2_PLACEMENT_3D('',#6446,#5308,#5309);
#4253=AXIS2_PLACEMENT_3D('',#6449,#5311,#5312);
#4254=AXIS2_PLACEMENT_3D('',#6450,#5313,#5314);
#4255=AXIS2_PLACEMENT_3D('',#6453,#5316,#5317);
#4256=AXIS2_PLACEMENT_3D('',#6454,#5318,#5319);
#4257=AXIS2_PLACEMENT_3D('',#6455,#5320,#5321);
#4258=AXIS2_PLACEMENT_3D('',#6456,#5322,#5323);
#4259=AXIS2_PLACEMENT_3D('',#6458,#5324,#5325);
#4260=AXIS2_PLACEMENT_3D('',#6460,#5326,#5327);
#4261=AXIS2_PLACEMENT_3D('',#6461,#5328,#5329);
#4262=AXIS2_PLACEMENT_3D('',#6463,#5330,#5331);
#4263=AXIS2_PLACEMENT_3D('',#6465,#5333,#5334);
#4264=AXIS2_PLACEMENT_3D('',#6467,#5335,#5336);
#4265=AXIS2_PLACEMENT_3D('',#6468,#5337,#5338);
#4266=AXIS2_PLACEMENT_3D('',#6471,#5340,#5341);
#4267=AXIS2_PLACEMENT_3D('',#6472,#5342,#5343);
#4268=AXIS2_PLACEMENT_3D('',#6475,#5345,#5346);
#4269=AXIS2_PLACEMENT_3D('',#6476,#5347,#5348);
#4270=AXIS2_PLACEMENT_3D('',#6477,#5349,#5350);
#4271=AXIS2_PLACEMENT_3D('',#6478,#5351,#5352);
#4272=AXIS2_PLACEMENT_3D('',#6480,#5353,#5354);
#4273=AXIS2_PLACEMENT_3D('',#6482,#5355,#5356);
#4274=AXIS2_PLACEMENT_3D('',#6483,#5357,#5358);
#4275=AXIS2_PLACEMENT_3D('',#6485,#5359,#5360);
#4276=AXIS2_PLACEMENT_3D('',#6487,#5362,#5363);
#4277=AXIS2_PLACEMENT_3D('',#6489,#5364,#5365);
#4278=AXIS2_PLACEMENT_3D('',#6490,#5366,#5367);
#4279=AXIS2_PLACEMENT_3D('',#6493,#5369,#5370);
#4280=AXIS2_PLACEMENT_3D('',#6494,#5371,#5372);
#4281=AXIS2_PLACEMENT_3D('',#6497,#5374,#5375);
#4282=AXIS2_PLACEMENT_3D('',#6498,#5376,#5377);
#4283=AXIS2_PLACEMENT_3D('',#6499,#5378,#5379);
#4284=AXIS2_PLACEMENT_3D('',#6500,#5380,#5381);
#4285=AXIS2_PLACEMENT_3D('',#6502,#5382,#5383);
#4286=AXIS2_PLACEMENT_3D('',#6504,#5384,#5385);
#4287=AXIS2_PLACEMENT_3D('',#6505,#5386,#5387);
#4288=AXIS2_PLACEMENT_3D('',#6507,#5388,#5389);
#4289=AXIS2_PLACEMENT_3D('',#6509,#5391,#5392);
#4290=AXIS2_PLACEMENT_3D('',#6511,#5393,#5394);
#4291=AXIS2_PLACEMENT_3D('',#6512,#5395,#5396);
#4292=AXIS2_PLACEMENT_3D('',#6515,#5398,#5399);
#4293=AXIS2_PLACEMENT_3D('',#6516,#5400,#5401);
#4294=AXIS2_PLACEMENT_3D('',#6519,#5403,#5404);
#4295=AXIS2_PLACEMENT_3D('',#6520,#5405,#5406);
#4296=AXIS2_PLACEMENT_3D('',#6521,#5407,#5408);
#4297=AXIS2_PLACEMENT_3D('',#6522,#5409,#5410);
#4298=AXIS2_PLACEMENT_3D('',#6523,#5411,#5412);
#4299=AXIS2_PLACEMENT_3D('',#6524,#5413,#5414);
#4300=AXIS2_PLACEMENT_3D('',#6525,#5415,#5416);
#4301=AXIS2_PLACEMENT_3D('',#6526,#5417,#5418);
#4302=AXIS2_PLACEMENT_3D('',#6527,#5419,#5420);
#4303=AXIS2_PLACEMENT_3D('',#6528,#5421,#5422);
#4304=AXIS2_PLACEMENT_3D('',#6530,#5423,#5424);
#4305=AXIS2_PLACEMENT_3D('',#6533,#5426,#5427);
#4306=AXIS2_PLACEMENT_3D('',#6534,#5428,#5429);
#4307=AXIS2_PLACEMENT_3D('',#6543,#5434,#5435);
#4308=AXIS2_PLACEMENT_3D('',#6549,#5439,#5440);
#4309=AXIS2_PLACEMENT_3D('',#6555,#5444,#5445);
#4310=AXIS2_PLACEMENT_3D('',#6556,#5446,#5447);
#4311=AXIS2_PLACEMENT_3D('',#6557,#5448,#5449);
#4312=AXIS2_PLACEMENT_3D('',#6558,#5450,#5451);
#4313=AXIS2_PLACEMENT_3D('',#6560,#5452,#5453);
#4314=AXIS2_PLACEMENT_3D('',#6561,#5454,#5455);
#4315=AXIS2_PLACEMENT_3D('',#6562,#5456,#5457);
#4316=AXIS2_PLACEMENT_3D('',#6565,#5459,#5460);
#4317=AXIS2_PLACEMENT_3D('',#6566,#5461,#5462);
#4318=AXIS2_PLACEMENT_3D('',#6567,#5463,#5464);
#4319=AXIS2_PLACEMENT_3D('',#6568,#5465,#5466);
#4320=AXIS2_PLACEMENT_3D('',#6570,#5467,#5468);
#4321=AXIS2_PLACEMENT_3D('',#6573,#5470,#5471);
#4322=AXIS2_PLACEMENT_3D('',#6574,#5472,#5473);
#4323=AXIS2_PLACEMENT_3D('',#6575,#5474,#5475);
#4324=AXIS2_PLACEMENT_3D('',#6576,#5476,#5477);
#4325=AXIS2_PLACEMENT_3D('',#6577,#5478,#5479);
#4326=AXIS2_PLACEMENT_3D('',#6578,#5480,#5481);
#4327=AXIS2_PLACEMENT_3D('',#6579,#5482,#5483);
#4328=AXIS2_PLACEMENT_3D('',#6580,#5484,#5485);
#4329=DIRECTION('axis',(0.,0.,1.));
#4330=DIRECTION('refdir',(1.,0.,0.));
#4331=DIRECTION('axis',(0.,0.,1.));
#4332=DIRECTION('refdir',(1.,0.,0.));
#4333=DIRECTION('axis',(0.,0.,1.));
#4334=DIRECTION('refdir',(1.,0.,0.));
#4335=DIRECTION('center_axis',(0.,0.,1.));
#4336=DIRECTION('ref_axis',(1.,0.,0.));
#4337=DIRECTION('center_axis',(0.,0.,1.));
#4338=DIRECTION('ref_axis',(1.,0.,0.));
#4339=DIRECTION('',(0.,0.,1.));
#4340=DIRECTION('center_axis',(0.,0.,-1.));
#4341=DIRECTION('ref_axis',(1.,0.,0.));
#4342=DIRECTION('center_axis',(0.,0.,1.));
#4343=DIRECTION('ref_axis',(1.,0.,0.));
#4344=DIRECTION('center_axis',(0.,0.,1.));
#4345=DIRECTION('ref_axis',(1.,0.,0.));
#4346=DIRECTION('',(0.,0.,1.));
#4347=DIRECTION('center_axis',(0.,0.,-1.));
#4348=DIRECTION('ref_axis',(1.,0.,0.));
#4349=DIRECTION('center_axis',(0.,0.,1.));
#4350=DIRECTION('ref_axis',(1.,0.,0.));
#4351=DIRECTION('center_axis',(0.,0.,1.));
#4352=DIRECTION('ref_axis',(1.,0.,0.));
#4353=DIRECTION('',(0.,0.,1.));
#4354=DIRECTION('center_axis',(0.,0.,-1.));
#4355=DIRECTION('ref_axis',(1.,0.,0.));
#4356=DIRECTION('center_axis',(0.,0.,1.));
#4357=DIRECTION('ref_axis',(1.,0.,0.));
#4358=DIRECTION('center_axis',(0.,0.,1.));
#4359=DIRECTION('ref_axis',(1.,0.,0.));
#4360=DIRECTION('',(0.,0.,1.));
#4361=DIRECTION('center_axis',(0.,0.,-1.));
#4362=DIRECTION('ref_axis',(1.,0.,0.));
#4363=DIRECTION('center_axis',(0.,0.,1.));
#4364=DIRECTION('ref_axis',(1.,0.,0.));
#4365=DIRECTION('center_axis',(0.,0.,1.));
#4366=DIRECTION('ref_axis',(1.,0.,0.));
#4367=DIRECTION('',(0.,0.,1.));
#4368=DIRECTION('center_axis',(0.,0.,-1.));
#4369=DIRECTION('ref_axis',(1.,0.,0.));
#4370=DIRECTION('center_axis',(0.,0.,1.));
#4371=DIRECTION('ref_axis',(1.,0.,0.));
#4372=DIRECTION('center_axis',(0.,0.,1.));
#4373=DIRECTION('ref_axis',(1.,0.,0.));
#4374=DIRECTION('',(0.,0.,1.));
#4375=DIRECTION('center_axis',(0.,0.,-1.));
#4376=DIRECTION('ref_axis',(1.,0.,0.));
#4377=DIRECTION('center_axis',(0.,0.,1.));
#4378=DIRECTION('ref_axis',(1.,0.,0.));
#4379=DIRECTION('center_axis',(0.,0.,1.));
#4380=DIRECTION('ref_axis',(1.,0.,0.));
#4381=DIRECTION('',(0.,0.,1.));
#4382=DIRECTION('center_axis',(0.,0.,-1.));
#4383=DIRECTION('ref_axis',(1.,0.,0.));
#4384=DIRECTION('center_axis',(0.,0.,1.));
#4385=DIRECTION('ref_axis',(1.,0.,0.));
#4386=DIRECTION('center_axis',(0.,0.,1.));
#4387=DIRECTION('ref_axis',(1.,0.,0.));
#4388=DIRECTION('',(0.,0.,1.));
#4389=DIRECTION('center_axis',(0.,0.,-1.));
#4390=DIRECTION('ref_axis',(1.,0.,0.));
#4391=DIRECTION('center_axis',(0.,0.,1.));
#4392=DIRECTION('ref_axis',(1.,0.,0.));
#4393=DIRECTION('center_axis',(0.,0.,1.));
#4394=DIRECTION('ref_axis',(1.,0.,0.));
#4395=DIRECTION('',(0.,0.,1.));
#4396=DIRECTION('center_axis',(0.,0.,-1.));
#4397=DIRECTION('ref_axis',(1.,0.,0.));
#4398=DIRECTION('center_axis',(0.,0.,1.));
#4399=DIRECTION('ref_axis',(1.,0.,0.));
#4400=DIRECTION('center_axis',(0.,0.,1.));
#4401=DIRECTION('ref_axis',(1.,0.,0.));
#4402=DIRECTION('',(0.,0.,1.));
#4403=DIRECTION('center_axis',(0.,0.,-1.));
#4404=DIRECTION('ref_axis',(1.,0.,0.));
#4405=DIRECTION('center_axis',(0.,0.,1.));
#4406=DIRECTION('ref_axis',(1.,0.,0.));
#4407=DIRECTION('center_axis',(0.,0.,1.));
#4408=DIRECTION('ref_axis',(1.,0.,0.));
#4409=DIRECTION('',(0.,0.,1.));
#4410=DIRECTION('center_axis',(0.,0.,-1.));
#4411=DIRECTION('ref_axis',(1.,0.,0.));
#4412=DIRECTION('center_axis',(0.,0.,1.));
#4413=DIRECTION('ref_axis',(1.,0.,0.));
#4414=DIRECTION('center_axis',(0.,0.,1.));
#4415=DIRECTION('ref_axis',(1.,0.,0.));
#4416=DIRECTION('',(0.,0.,1.));
#4417=DIRECTION('center_axis',(0.,0.,-1.));
#4418=DIRECTION('ref_axis',(1.,0.,0.));
#4419=DIRECTION('center_axis',(0.,0.,1.));
#4420=DIRECTION('ref_axis',(1.,0.,0.));
#4421=DIRECTION('center_axis',(0.,0.,1.));
#4422=DIRECTION('ref_axis',(1.,0.,0.));
#4423=DIRECTION('',(0.,0.,1.));
#4424=DIRECTION('center_axis',(0.,0.,-1.));
#4425=DIRECTION('ref_axis',(1.,0.,0.));
#4426=DIRECTION('center_axis',(0.,0.,1.));
#4427=DIRECTION('ref_axis',(1.,0.,0.));
#4428=DIRECTION('center_axis',(0.,0.,1.));
#4429=DIRECTION('ref_axis',(1.,0.,0.));
#4430=DIRECTION('',(0.,0.,1.));
#4431=DIRECTION('center_axis',(0.,0.,-1.));
#4432=DIRECTION('ref_axis',(1.,0.,0.));
#4433=DIRECTION('center_axis',(0.,1.,0.));
#4434=DIRECTION('ref_axis',(-1.,0.,0.));
#4435=DIRECTION('',(-1.,0.,0.));
#4436=DIRECTION('',(0.,0.,1.));
#4437=DIRECTION('',(-1.,0.,0.));
#4438=DIRECTION('',(0.,0.,1.));
#4439=DIRECTION('center_axis',(1.,0.,0.));
#4440=DIRECTION('ref_axis',(0.,1.,0.));
#4441=DIRECTION('',(0.,1.,0.));
#4442=DIRECTION('',(0.,1.,0.));
#4443=DIRECTION('',(0.,0.,1.));
#4444=DIRECTION('center_axis',(0.,-1.,0.));
#4445=DIRECTION('ref_axis',(1.,0.,0.));
#4446=DIRECTION('',(1.,0.,0.));
#4447=DIRECTION('',(1.,0.,0.));
#4448=DIRECTION('',(0.,0.,1.));
#4449=DIRECTION('center_axis',(-1.,0.,0.));
#4450=DIRECTION('ref_axis',(0.,-1.,0.));
#4451=DIRECTION('',(0.,-1.,0.));
#4452=DIRECTION('',(0.,-1.,0.));
#4453=DIRECTION('center_axis',(0.,0.,1.));
#4454=DIRECTION('ref_axis',(1.,0.,0.));
#4455=DIRECTION('center_axis',(0.,0.,1.));
#4456=DIRECTION('ref_axis',(1.,0.,0.));
#4457=DIRECTION('axis',(0.,0.,1.));
#4458=DIRECTION('refdir',(1.,0.,0.));
#4459=DIRECTION('center_axis',(0.,0.,1.));
#4460=DIRECTION('ref_axis',(1.,0.,0.));
#4461=DIRECTION('center_axis',(0.,0.,1.));
#4462=DIRECTION('ref_axis',(1.,0.,0.));
#4463=DIRECTION('',(0.,0.,-1.));
#4464=DIRECTION('center_axis',(0.,0.,1.));
#4465=DIRECTION('ref_axis',(1.,0.,0.));
#4466=DIRECTION('center_axis',(0.,0.,1.));
#4467=DIRECTION('ref_axis',(1.,0.,0.));
#4468=DIRECTION('center_axis',(0.,0.,1.));
#4469=DIRECTION('ref_axis',(1.,0.,0.));
#4470=DIRECTION('axis',(0.,0.,1.));
#4471=DIRECTION('refdir',(1.,0.,0.));
#4472=DIRECTION('center_axis',(0.,0.,1.));
#4473=DIRECTION('ref_axis',(1.,0.,0.));
#4474=DIRECTION('center_axis',(0.,0.,1.));
#4475=DIRECTION('ref_axis',(1.,0.,0.));
#4476=DIRECTION('',(0.,0.,-1.));
#4477=DIRECTION('center_axis',(0.,0.,1.));
#4478=DIRECTION('ref_axis',(1.,0.,0.));
#4479=DIRECTION('center_axis',(0.,0.,1.));
#4480=DIRECTION('ref_axis',(1.,0.,0.));
#4481=DIRECTION('center_axis',(0.,0.,1.));
#4482=DIRECTION('ref_axis',(1.,0.,0.));
#4483=DIRECTION('axis',(0.,0.,1.));
#4484=DIRECTION('refdir',(1.,0.,0.));
#4485=DIRECTION('center_axis',(0.,0.,1.));
#4486=DIRECTION('ref_axis',(1.,0.,0.));
#4487=DIRECTION('center_axis',(0.,0.,1.));
#4488=DIRECTION('ref_axis',(1.,0.,0.));
#4489=DIRECTION('',(0.,0.,-1.));
#4490=DIRECTION('center_axis',(0.,0.,1.));
#4491=DIRECTION('ref_axis',(1.,0.,0.));
#4492=DIRECTION('center_axis',(0.,0.,1.));
#4493=DIRECTION('ref_axis',(1.,0.,0.));
#4494=DIRECTION('center_axis',(0.,0.,1.));
#4495=DIRECTION('ref_axis',(1.,0.,0.));
#4496=DIRECTION('axis',(0.,0.,1.));
#4497=DIRECTION('refdir',(1.,0.,0.));
#4498=DIRECTION('center_axis',(0.,0.,1.));
#4499=DIRECTION('ref_axis',(1.,0.,0.));
#4500=DIRECTION('center_axis',(0.,0.,1.));
#4501=DIRECTION('ref_axis',(1.,0.,0.));
#4502=DIRECTION('',(0.,0.,-1.));
#4503=DIRECTION('center_axis',(0.,0.,1.));
#4504=DIRECTION('ref_axis',(1.,0.,0.));
#4505=DIRECTION('center_axis',(0.,0.,1.));
#4506=DIRECTION('ref_axis',(1.,0.,0.));
#4507=DIRECTION('center_axis',(0.,0.,1.));
#4508=DIRECTION('ref_axis',(1.,0.,0.));
#4509=DIRECTION('axis',(0.,0.,1.));
#4510=DIRECTION('refdir',(1.,0.,0.));
#4511=DIRECTION('center_axis',(0.,0.,1.));
#4512=DIRECTION('ref_axis',(1.,0.,0.));
#4513=DIRECTION('center_axis',(0.,0.,1.));
#4514=DIRECTION('ref_axis',(1.,0.,0.));
#4515=DIRECTION('',(0.,0.,1.));
#4516=DIRECTION('center_axis',(0.,0.,-1.));
#4517=DIRECTION('ref_axis',(1.,0.,0.));
#4518=DIRECTION('center_axis',(0.,0.,1.));
#4519=DIRECTION('ref_axis',(1.,0.,0.));
#4520=DIRECTION('center_axis',(0.,0.,1.));
#4521=DIRECTION('ref_axis',(1.,0.,0.));
#4522=DIRECTION('center_axis',(0.,0.,1.));
#4523=DIRECTION('ref_axis',(1.,0.,0.));
#4524=DIRECTION('center_axis',(0.,0.,1.));
#4525=DIRECTION('ref_axis',(1.,0.,0.));
#4526=DIRECTION('',(0.,0.,1.));
#4527=DIRECTION('center_axis',(0.,0.,-1.));
#4528=DIRECTION('ref_axis',(1.,0.,0.));
#4529=DIRECTION('center_axis',(0.,0.,1.));
#4530=DIRECTION('ref_axis',(1.,0.,0.));
#4531=DIRECTION('center_axis',(0.,0.,1.));
#4532=DIRECTION('ref_axis',(1.,0.,0.));
#4533=DIRECTION('center_axis',(0.,0.,1.));
#4534=DIRECTION('ref_axis',(1.,0.,0.));
#4535=DIRECTION('center_axis',(0.,0.,1.));
#4536=DIRECTION('ref_axis',(1.,0.,0.));
#4537=DIRECTION('',(0.,0.,1.));
#4538=DIRECTION('center_axis',(0.,0.,-1.));
#4539=DIRECTION('ref_axis',(1.,0.,0.));
#4540=DIRECTION('center_axis',(0.,0.,1.));
#4541=DIRECTION('ref_axis',(1.,0.,0.));
#4542=DIRECTION('center_axis',(0.,0.,1.));
#4543=DIRECTION('ref_axis',(1.,0.,0.));
#4544=DIRECTION('center_axis',(0.,0.,1.));
#4545=DIRECTION('ref_axis',(1.,0.,0.));
#4546=DIRECTION('center_axis',(0.,0.,1.));
#4547=DIRECTION('ref_axis',(1.,0.,0.));
#4548=DIRECTION('',(0.,0.,1.));
#4549=DIRECTION('center_axis',(0.,0.,-1.));
#4550=DIRECTION('ref_axis',(1.,0.,0.));
#4551=DIRECTION('center_axis',(0.,0.,1.));
#4552=DIRECTION('ref_axis',(1.,0.,0.));
#4553=DIRECTION('center_axis',(0.,0.,1.));
#4554=DIRECTION('ref_axis',(1.,0.,0.));
#4555=DIRECTION('center_axis',(0.,0.,1.));
#4556=DIRECTION('ref_axis',(1.,0.,0.));
#4557=DIRECTION('center_axis',(0.,0.,1.));
#4558=DIRECTION('ref_axis',(1.,0.,0.));
#4559=DIRECTION('',(0.,0.,1.));
#4560=DIRECTION('center_axis',(0.,0.,1.));
#4561=DIRECTION('ref_axis',(1.,0.,0.));
#4562=DIRECTION('center_axis',(0.,0.,1.));
#4563=DIRECTION('ref_axis',(1.,0.,0.));
#4564=DIRECTION('',(0.,0.,1.));
#4565=DIRECTION('center_axis',(0.,0.,1.));
#4566=DIRECTION('ref_axis',(1.,0.,0.));
#4567=DIRECTION('center_axis',(0.,0.,1.));
#4568=DIRECTION('ref_axis',(1.,0.,0.));
#4569=DIRECTION('',(0.,0.,1.));
#4570=DIRECTION('center_axis',(0.,0.,1.));
#4571=DIRECTION('ref_axis',(1.,0.,0.));
#4572=DIRECTION('center_axis',(0.,0.,1.));
#4573=DIRECTION('ref_axis',(1.,0.,0.));
#4574=DIRECTION('',(0.,0.,1.));
#4575=DIRECTION('center_axis',(0.,-1.,0.));
#4576=DIRECTION('ref_axis',(1.,0.,0.));
#4577=DIRECTION('',(-1.,0.,0.));
#4578=DIRECTION('',(0.,0.,1.));
#4579=DIRECTION('',(1.,0.,0.));
#4580=DIRECTION('',(0.,0.,1.));
#4581=DIRECTION('center_axis',(-1.,0.,0.));
#4582=DIRECTION('ref_axis',(0.,-1.,0.));
#4583=DIRECTION('',(0.,1.,0.));
#4584=DIRECTION('',(0.,-1.,0.));
#4585=DIRECTION('',(0.,0.,1.));
#4586=DIRECTION('center_axis',(0.,1.,0.));
#4587=DIRECTION('ref_axis',(-1.,0.,0.));
#4588=DIRECTION('',(1.,0.,0.));
#4589=DIRECTION('',(-1.,0.,0.));
#4590=DIRECTION('',(0.,0.,1.));
#4591=DIRECTION('center_axis',(1.,0.,0.));
#4592=DIRECTION('ref_axis',(0.,1.,0.));
#4593=DIRECTION('',(0.,-1.,0.));
#4594=DIRECTION('',(0.,1.,0.));
#4595=DIRECTION('center_axis',(0.,0.,1.));
#4596=DIRECTION('ref_axis',(1.,0.,0.));
#4597=DIRECTION('center_axis',(0.,1.,0.));
#4598=DIRECTION('ref_axis',(-1.,0.,0.));
#4599=DIRECTION('',(-1.,0.,0.));
#4600=DIRECTION('',(0.,0.,1.));
#4601=DIRECTION('',(-1.,0.,0.));
#4602=DIRECTION('',(0.,0.,1.));
#4603=DIRECTION('center_axis',(1.,0.,0.));
#4604=DIRECTION('ref_axis',(0.,1.,0.));
#4605=DIRECTION('',(0.,1.,0.));
#4606=DIRECTION('',(0.,1.,0.));
#4607=DIRECTION('',(0.,0.,1.));
#4608=DIRECTION('center_axis',(0.,-1.,0.));
#4609=DIRECTION('ref_axis',(1.,0.,0.));
#4610=DIRECTION('',(1.,0.,0.));
#4611=DIRECTION('',(1.,0.,0.));
#4612=DIRECTION('',(0.,0.,1.));
#4613=DIRECTION('center_axis',(-1.,0.,0.));
#4614=DIRECTION('ref_axis',(0.,-1.,0.));
#4615=DIRECTION('',(0.,-1.,0.));
#4616=DIRECTION('',(0.,-1.,0.));
#4617=DIRECTION('center_axis',(0.,0.,1.));
#4618=DIRECTION('ref_axis',(1.,0.,0.));
#4619=DIRECTION('center_axis',(0.,0.,1.));
#4620=DIRECTION('ref_axis',(1.,0.,0.));
#4621=DIRECTION('axis',(0.,0.,1.));
#4622=DIRECTION('refdir',(1.,0.,0.));
#4623=DIRECTION('center_axis',(0.,1.,0.));
#4624=DIRECTION('ref_axis',(-1.,0.,0.));
#4625=DIRECTION('',(-1.,0.,0.));
#4626=DIRECTION('',(0.,0.,1.));
#4627=DIRECTION('',(-1.,0.,0.));
#4628=DIRECTION('',(0.,0.,1.));
#4629=DIRECTION('center_axis',(1.,0.,0.));
#4630=DIRECTION('ref_axis',(0.,1.,0.));
#4631=DIRECTION('',(0.,1.,0.));
#4632=DIRECTION('',(0.,1.,0.));
#4633=DIRECTION('',(0.,0.,1.));
#4634=DIRECTION('center_axis',(0.,-1.,0.));
#4635=DIRECTION('ref_axis',(1.,0.,0.));
#4636=DIRECTION('',(1.,0.,0.));
#4637=DIRECTION('',(1.,0.,0.));
#4638=DIRECTION('',(0.,0.,1.));
#4639=DIRECTION('center_axis',(-1.,0.,0.));
#4640=DIRECTION('ref_axis',(0.,-1.,0.));
#4641=DIRECTION('',(0.,-1.,0.));
#4642=DIRECTION('',(0.,-1.,0.));
#4643=DIRECTION('center_axis',(0.,0.,1.));
#4644=DIRECTION('ref_axis',(1.,0.,0.));
#4645=DIRECTION('center_axis',(0.,0.,1.));
#4646=DIRECTION('ref_axis',(1.,0.,0.));
#4647=DIRECTION('axis',(0.,0.,1.));
#4648=DIRECTION('refdir',(1.,0.,0.));
#4649=DIRECTION('center_axis',(0.,0.,1.));
#4650=DIRECTION('ref_axis',(1.,0.,0.));
#4651=DIRECTION('center_axis',(0.,0.,1.));
#4652=DIRECTION('ref_axis',(1.,0.,0.));
#4653=DIRECTION('',(0.,0.,1.));
#4654=DIRECTION('center_axis',(0.,0.,-1.));
#4655=DIRECTION('ref_axis',(1.,0.,0.));
#4656=DIRECTION('center_axis',(0.,0.,1.));
#4657=DIRECTION('ref_axis',(1.,0.,0.));
#4658=DIRECTION('center_axis',(0.,0.,1.));
#4659=DIRECTION('ref_axis',(1.,0.,0.));
#4660=DIRECTION('center_axis',(0.,0.,1.));
#4661=DIRECTION('ref_axis',(1.,0.,0.));
#4662=DIRECTION('center_axis',(0.,0.,1.));
#4663=DIRECTION('ref_axis',(1.,0.,0.));
#4664=DIRECTION('',(0.,0.,1.));
#4665=DIRECTION('center_axis',(0.,0.,1.));
#4666=DIRECTION('ref_axis',(1.,0.,0.));
#4667=DIRECTION('center_axis',(0.,0.,1.));
#4668=DIRECTION('ref_axis',(1.,0.,0.));
#4669=DIRECTION('',(0.,0.,1.));
#4670=DIRECTION('center_axis',(0.,0.,-1.));
#4671=DIRECTION('ref_axis',(1.,0.,0.));
#4672=DIRECTION('center_axis',(1.,0.,0.));
#4673=DIRECTION('ref_axis',(0.,0.,-1.));
#4674=DIRECTION('center_axis',(1.,0.,0.));
#4675=DIRECTION('ref_axis',(0.,0.,-1.));
#4676=DIRECTION('',(1.,0.,0.));
#4677=DIRECTION('center_axis',(-1.,0.,0.));
#4678=DIRECTION('ref_axis',(0.,0.,-1.));
#4679=DIRECTION('center_axis',(0.,0.,1.));
#4680=DIRECTION('ref_axis',(0.,-1.,0.));
#4681=DIRECTION('',(0.,-1.,0.));
#4682=DIRECTION('',(1.,0.,0.));
#4683=DIRECTION('',(0.,-1.,0.));
#4684=DIRECTION('',(1.,0.,0.));
#4685=DIRECTION('center_axis',(0.,1.,0.));
#4686=DIRECTION('ref_axis',(0.,0.,1.));
#4687=DIRECTION('',(0.,0.,1.));
#4688=DIRECTION('',(0.,0.,1.));
#4689=DIRECTION('',(1.,0.,0.));
#4690=DIRECTION('center_axis',(0.,0.,1.));
#4691=DIRECTION('ref_axis',(0.,-1.,0.));
#4692=DIRECTION('',(0.,-1.,0.));
#4693=DIRECTION('',(0.,-1.,0.));
#4694=DIRECTION('',(1.,0.,0.));
#4695=DIRECTION('center_axis',(0.,1.,0.));
#4696=DIRECTION('ref_axis',(0.,0.,1.));
#4697=DIRECTION('',(0.,0.,1.));
#4698=DIRECTION('',(0.,0.,1.));
#4699=DIRECTION('',(1.,0.,0.));
#4700=DIRECTION('center_axis',(0.,0.,-1.));
#4701=DIRECTION('ref_axis',(0.,1.,0.));
#4702=DIRECTION('',(0.,1.,0.));
#4703=DIRECTION('',(0.,1.,0.));
#4704=DIRECTION('',(1.,0.,0.));
#4705=DIRECTION('center_axis',(0.,-1.,0.));
#4706=DIRECTION('ref_axis',(0.,0.,-1.));
#4707=DIRECTION('',(0.,0.,-1.));
#4708=DIRECTION('',(0.,0.,-1.));
#4709=DIRECTION('center_axis',(1.,0.,0.));
#4710=DIRECTION('ref_axis',(0.,0.,-1.));
#4711=DIRECTION('center_axis',(1.,0.,0.));
#4712=DIRECTION('ref_axis',(0.,0.,-1.));
#4713=DIRECTION('axis',(0.,0.,1.));
#4714=DIRECTION('refdir',(1.,0.,0.));
#4715=DIRECTION('center_axis',(0.,0.,1.));
#4716=DIRECTION('ref_axis',(1.,0.,0.));
#4717=DIRECTION('center_axis',(0.,0.,1.));
#4718=DIRECTION('ref_axis',(1.,0.,0.));
#4719=DIRECTION('',(0.,0.,1.));
#4720=DIRECTION('center_axis',(0.,0.,-1.));
#4721=DIRECTION('ref_axis',(1.,0.,0.));
#4722=DIRECTION('center_axis',(0.,0.,1.));
#4723=DIRECTION('ref_axis',(1.,0.,0.));
#4724=DIRECTION('center_axis',(0.,0.,1.));
#4725=DIRECTION('ref_axis',(1.,0.,0.));
#4726=DIRECTION('center_axis',(0.,0.,1.));
#4727=DIRECTION('ref_axis',(1.,0.,0.));
#4728=DIRECTION('center_axis',(0.,0.,1.));
#4729=DIRECTION('ref_axis',(1.,0.,0.));
#4730=DIRECTION('',(0.,0.,1.));
#4731=DIRECTION('center_axis',(0.,0.,1.));
#4732=DIRECTION('ref_axis',(1.,0.,0.));
#4733=DIRECTION('center_axis',(0.,0.,1.));
#4734=DIRECTION('ref_axis',(1.,0.,0.));
#4735=DIRECTION('',(0.,0.,1.));
#4736=DIRECTION('center_axis',(0.,0.,-1.));
#4737=DIRECTION('ref_axis',(1.,0.,0.));
#4738=DIRECTION('center_axis',(1.,0.,0.));
#4739=DIRECTION('ref_axis',(0.,0.,-1.));
#4740=DIRECTION('center_axis',(1.,0.,0.));
#4741=DIRECTION('ref_axis',(0.,0.,-1.));
#4742=DIRECTION('',(1.,0.,0.));
#4743=DIRECTION('center_axis',(-1.,0.,0.));
#4744=DIRECTION('ref_axis',(0.,0.,-1.));
#4745=DIRECTION('center_axis',(0.,0.,1.));
#4746=DIRECTION('ref_axis',(0.,-1.,0.));
#4747=DIRECTION('',(0.,-1.,0.));
#4748=DIRECTION('',(1.,0.,0.));
#4749=DIRECTION('',(0.,-1.,0.));
#4750=DIRECTION('',(1.,0.,0.));
#4751=DIRECTION('center_axis',(0.,1.,0.));
#4752=DIRECTION('ref_axis',(0.,0.,1.));
#4753=DIRECTION('',(0.,0.,1.));
#4754=DIRECTION('',(0.,0.,1.));
#4755=DIRECTION('',(1.,0.,0.));
#4756=DIRECTION('center_axis',(0.,0.,1.));
#4757=DIRECTION('ref_axis',(0.,-1.,0.));
#4758=DIRECTION('',(0.,-1.,0.));
#4759=DIRECTION('',(0.,-1.,0.));
#4760=DIRECTION('',(1.,0.,0.));
#4761=DIRECTION('center_axis',(0.,1.,0.));
#4762=DIRECTION('ref_axis',(0.,0.,1.));
#4763=DIRECTION('',(0.,0.,1.));
#4764=DIRECTION('',(0.,0.,1.));
#4765=DIRECTION('',(1.,0.,0.));
#4766=DIRECTION('center_axis',(0.,0.,-1.));
#4767=DIRECTION('ref_axis',(0.,1.,0.));
#4768=DIRECTION('',(0.,1.,0.));
#4769=DIRECTION('',(0.,1.,0.));
#4770=DIRECTION('',(1.,0.,0.));
#4771=DIRECTION('center_axis',(0.,-1.,0.));
#4772=DIRECTION('ref_axis',(0.,0.,-1.));
#4773=DIRECTION('',(0.,0.,-1.));
#4774=DIRECTION('',(0.,0.,-1.));
#4775=DIRECTION('center_axis',(1.,0.,0.));
#4776=DIRECTION('ref_axis',(0.,0.,-1.));
#4777=DIRECTION('center_axis',(1.,0.,0.));
#4778=DIRECTION('ref_axis',(0.,0.,-1.));
#4779=DIRECTION('axis',(0.,0.,1.));
#4780=DIRECTION('refdir',(1.,0.,0.));
#4781=DIRECTION('center_axis',(1.,0.,0.));
#4782=DIRECTION('ref_axis',(0.,0.,-1.));
#4783=DIRECTION('center_axis',(1.,0.,0.));
#4784=DIRECTION('ref_axis',(0.,0.,-1.));
#4785=DIRECTION('',(1.,0.,0.));
#4786=DIRECTION('center_axis',(-1.,0.,0.));
#4787=DIRECTION('ref_axis',(0.,0.,-1.));
#4788=DIRECTION('center_axis',(1.,0.,0.));
#4789=DIRECTION('ref_axis',(0.,0.,-1.));
#4790=DIRECTION('center_axis',(1.,0.,0.));
#4791=DIRECTION('ref_axis',(0.,0.,-1.));
#4792=DIRECTION('center_axis',(1.,0.,0.));
#4793=DIRECTION('ref_axis',(0.,0.,-1.));
#4794=DIRECTION('',(1.,0.,0.));
#4795=DIRECTION('center_axis',(1.,0.,0.));
#4796=DIRECTION('ref_axis',(0.,0.,-1.));
#4797=DIRECTION('center_axis',(1.,0.,0.));
#4798=DIRECTION('ref_axis',(0.,0.,-1.));
#4799=DIRECTION('center_axis',(1.,0.,0.));
#4800=DIRECTION('ref_axis',(0.,0.,-1.));
#4801=DIRECTION('center_axis',(1.,0.,0.));
#4802=DIRECTION('ref_axis',(0.,0.,-1.));
#4803=DIRECTION('',(-1.,0.,0.));
#4804=DIRECTION('center_axis',(1.,0.,0.));
#4805=DIRECTION('ref_axis',(0.,0.,-1.));
#4806=DIRECTION('center_axis',(1.,0.,0.));
#4807=DIRECTION('ref_axis',(0.,0.,-1.));
#4808=DIRECTION('center_axis',(1.,0.,0.));
#4809=DIRECTION('ref_axis',(0.,0.,-1.));
#4810=DIRECTION('axis',(0.,0.,1.));
#4811=DIRECTION('refdir',(1.,0.,0.));
#4812=DIRECTION('center_axis',(1.,0.,0.));
#4813=DIRECTION('ref_axis',(0.,0.,-1.));
#4814=DIRECTION('center_axis',(-1.,0.,0.));
#4815=DIRECTION('ref_axis',(0.,0.,-1.));
#4816=DIRECTION('',(-1.,0.,0.));
#4817=DIRECTION('center_axis',(-1.,0.,0.));
#4818=DIRECTION('ref_axis',(0.,0.,-1.));
#4819=DIRECTION('center_axis',(1.,0.,0.));
#4820=DIRECTION('ref_axis',(0.,0.,-1.));
#4821=DIRECTION('center_axis',(1.,0.,0.));
#4822=DIRECTION('ref_axis',(0.,0.,-1.));
#4823=DIRECTION('',(-1.,0.,0.));
#4824=DIRECTION('center_axis',(1.,0.,0.));
#4825=DIRECTION('ref_axis',(0.,0.,-1.));
#4826=DIRECTION('center_axis',(1.,0.,0.));
#4827=DIRECTION('ref_axis',(0.,0.,-1.));
#4828=DIRECTION('center_axis',(1.,0.,0.));
#4829=DIRECTION('ref_axis',(0.,0.,-1.));
#4830=DIRECTION('axis',(0.,0.,1.));
#4831=DIRECTION('refdir',(1.,0.,0.));
#4832=DIRECTION('center_axis',(1.,0.,0.));
#4833=DIRECTION('ref_axis',(0.,0.,-1.));
#4834=DIRECTION('center_axis',(-1.,0.,0.));
#4835=DIRECTION('ref_axis',(0.,0.,-1.));
#4836=DIRECTION('',(-1.,0.,0.));
#4837=DIRECTION('center_axis',(-1.,0.,0.));
#4838=DIRECTION('ref_axis',(0.,0.,-1.));
#4839=DIRECTION('center_axis',(1.,0.,0.));
#4840=DIRECTION('ref_axis',(0.,0.,-1.));
#4841=DIRECTION('center_axis',(1.,0.,0.));
#4842=DIRECTION('ref_axis',(0.,0.,-1.));
#4843=DIRECTION('',(-1.,0.,0.));
#4844=DIRECTION('center_axis',(1.,0.,0.));
#4845=DIRECTION('ref_axis',(0.,0.,-1.));
#4846=DIRECTION('center_axis',(1.,0.,0.));
#4847=DIRECTION('ref_axis',(0.,0.,-1.));
#4848=DIRECTION('center_axis',(1.,0.,0.));
#4849=DIRECTION('ref_axis',(0.,0.,-1.));
#4850=DIRECTION('axis',(0.,0.,1.));
#4851=DIRECTION('refdir',(1.,0.,0.));
#4852=DIRECTION('center_axis',(0.,0.,1.));
#4853=DIRECTION('ref_axis',(1.,0.,0.));
#4854=DIRECTION('center_axis',(0.,0.,1.));
#4855=DIRECTION('ref_axis',(1.,0.,0.));
#4856=DIRECTION('',(0.,0.,1.));
#4857=DIRECTION('center_axis',(0.,0.,-1.));
#4858=DIRECTION('ref_axis',(1.,0.,0.));
#4859=DIRECTION('center_axis',(0.,0.,1.));
#4860=DIRECTION('ref_axis',(1.,0.,0.));
#4861=DIRECTION('center_axis',(0.,0.,1.));
#4862=DIRECTION('ref_axis',(1.,0.,0.));
#4863=DIRECTION('center_axis',(0.,0.,1.));
#4864=DIRECTION('ref_axis',(1.,0.,0.));
#4865=DIRECTION('center_axis',(0.,0.,1.));
#4866=DIRECTION('ref_axis',(1.,0.,0.));
#4867=DIRECTION('center_axis',(0.,0.,1.));
#4868=DIRECTION('ref_axis',(1.,0.,0.));
#4869=DIRECTION('center_axis',(0.,0.,1.));
#4870=DIRECTION('ref_axis',(1.,0.,0.));
#4871=DIRECTION('',(0.,0.,1.));
#4872=DIRECTION('center_axis',(0.,0.,-1.));
#4873=DIRECTION('ref_axis',(1.,0.,0.));
#4874=DIRECTION('',(0.,0.,-1.));
#4875=DIRECTION('',(0.,0.,1.));
#4876=DIRECTION('center_axis',(0.,0.,-1.));
#4877=DIRECTION('ref_axis',(1.,0.,0.));
#4878=DIRECTION('center_axis',(0.,0.,1.));
#4879=DIRECTION('ref_axis',(1.,0.,0.));
#4880=DIRECTION('center_axis',(0.,0.,1.));
#4881=DIRECTION('ref_axis',(1.,0.,0.));
#4882=DIRECTION('center_axis',(0.,0.,1.));
#4883=DIRECTION('ref_axis',(1.,0.,0.));
#4884=DIRECTION('center_axis',(0.,0.,1.));
#4885=DIRECTION('ref_axis',(1.,0.,0.));
#4886=DIRECTION('center_axis',(0.,0.,1.));
#4887=DIRECTION('ref_axis',(1.,0.,0.));
#4888=DIRECTION('',(0.,0.,1.));
#4889=DIRECTION('center_axis',(0.,0.,-1.));
#4890=DIRECTION('ref_axis',(1.,0.,0.));
#4891=DIRECTION('',(0.,0.,-1.));
#4892=DIRECTION('',(0.,0.,1.));
#4893=DIRECTION('center_axis',(0.,0.,-1.));
#4894=DIRECTION('ref_axis',(1.,0.,0.));
#4895=DIRECTION('center_axis',(0.,0.,1.));
#4896=DIRECTION('ref_axis',(1.,0.,0.));
#4897=DIRECTION('center_axis',(0.,0.,1.));
#4898=DIRECTION('ref_axis',(1.,0.,0.));
#4899=DIRECTION('',(0.,0.,-1.));
#4900=DIRECTION('center_axis',(0.,0.,1.));
#4901=DIRECTION('ref_axis',(1.,0.,0.));
#4902=DIRECTION('center_axis',(0.,0.,1.));
#4903=DIRECTION('ref_axis',(1.,0.,0.));
#4904=DIRECTION('center_axis',(0.,0.,1.));
#4905=DIRECTION('ref_axis',(1.,0.,0.));
#4906=DIRECTION('center_axis',(0.,0.,1.));
#4907=DIRECTION('ref_axis',(1.,0.,0.));
#4908=DIRECTION('center_axis',(0.,0.,1.));
#4909=DIRECTION('ref_axis',(1.,0.,0.));
#4910=DIRECTION('center_axis',(0.,0.,1.));
#4911=DIRECTION('ref_axis',(1.,0.,0.));
#4912=DIRECTION('',(0.,0.,-1.));
#4913=DIRECTION('center_axis',(0.,0.,1.));
#4914=DIRECTION('ref_axis',(1.,0.,0.));
#4915=DIRECTION('center_axis',(0.,0.,1.));
#4916=DIRECTION('ref_axis',(1.,0.,0.));
#4917=DIRECTION('center_axis',(0.,0.,1.));
#4918=DIRECTION('ref_axis',(1.,0.,0.));
#4919=DIRECTION('',(0.,0.,-1.));
#4920=DIRECTION('center_axis',(0.,0.,-1.));
#4921=DIRECTION('ref_axis',(1.,0.,0.));
#4922=DIRECTION('center_axis',(0.,0.,1.));
#4923=DIRECTION('ref_axis',(1.,0.,0.));
#4924=DIRECTION('center_axis',(0.,0.,1.));
#4925=DIRECTION('ref_axis',(1.,0.,0.));
#4926=DIRECTION('center_axis',(0.,0.,1.));
#4927=DIRECTION('ref_axis',(1.,0.,0.));
#4928=DIRECTION('axis',(0.,0.,1.));
#4929=DIRECTION('refdir',(1.,0.,0.));
#4930=DIRECTION('center_axis',(0.,0.,1.));
#4931=DIRECTION('ref_axis',(1.,0.,0.));
#4932=DIRECTION('center_axis',(0.,0.,-1.));
#4933=DIRECTION('ref_axis',(1.,0.,0.));
#4934=DIRECTION('',(0.,0.,-1.));
#4935=DIRECTION('center_axis',(0.,0.,-1.));
#4936=DIRECTION('ref_axis',(1.,0.,0.));
#4937=DIRECTION('center_axis',(0.,0.,1.));
#4938=DIRECTION('ref_axis',(1.,0.,0.));
#4939=DIRECTION('center_axis',(0.,0.,1.));
#4940=DIRECTION('ref_axis',(1.,0.,0.));
#4941=DIRECTION('',(0.,0.,-1.));
#4942=DIRECTION('center_axis',(0.,0.,1.));
#4943=DIRECTION('ref_axis',(1.,0.,0.));
#4944=DIRECTION('center_axis',(0.,0.,1.));
#4945=DIRECTION('ref_axis',(1.,0.,0.));
#4946=DIRECTION('center_axis',(0.,0.,1.));
#4947=DIRECTION('ref_axis',(1.,0.,0.));
#4948=DIRECTION('axis',(0.,0.,1.));
#4949=DIRECTION('refdir',(1.,0.,0.));
#4950=DIRECTION('center_axis',(0.,0.,1.));
#4951=DIRECTION('ref_axis',(1.,0.,0.));
#4952=DIRECTION('center_axis',(0.,0.,-1.));
#4953=DIRECTION('ref_axis',(1.,0.,0.));
#4954=DIRECTION('',(0.,0.,-1.));
#4955=DIRECTION('center_axis',(0.,0.,-1.));
#4956=DIRECTION('ref_axis',(1.,0.,0.));
#4957=DIRECTION('center_axis',(0.,0.,1.));
#4958=DIRECTION('ref_axis',(1.,0.,0.));
#4959=DIRECTION('center_axis',(0.,0.,1.));
#4960=DIRECTION('ref_axis',(1.,0.,0.));
#4961=DIRECTION('',(0.,0.,-1.));
#4962=DIRECTION('center_axis',(0.,0.,1.));
#4963=DIRECTION('ref_axis',(1.,0.,0.));
#4964=DIRECTION('center_axis',(0.,0.,1.));
#4965=DIRECTION('ref_axis',(1.,0.,0.));
#4966=DIRECTION('center_axis',(0.,0.,1.));
#4967=DIRECTION('ref_axis',(1.,0.,0.));
#4968=DIRECTION('axis',(0.,0.,1.));
#4969=DIRECTION('refdir',(1.,0.,0.));
#4970=DIRECTION('center_axis',(0.866025403784439,0.,-0.5));
#4971=DIRECTION('ref_axis',(0.5,0.,0.866025403784439));
#4972=DIRECTION('',(-0.5,0.,-0.866025403784439));
#4973=DIRECTION('',(0.,-1.,0.));
#4974=DIRECTION('',(0.5,0.,0.866025403784439));
#4975=DIRECTION('',(0.,-1.,0.));
#4976=DIRECTION('center_axis',(1.20185167898973E-16,0.,-1.));
#4977=DIRECTION('ref_axis',(1.,0.,1.20185167898973E-16));
#4978=DIRECTION('',(-1.,0.,-1.20185167898973E-16));
#4979=DIRECTION('',(0.,-1.,0.));
#4980=DIRECTION('',(1.,0.,1.20185167898973E-16));
#4981=DIRECTION('center_axis',(-0.866025403784439,0.,-0.5));
#4982=DIRECTION('ref_axis',(0.5,0.,-0.866025403784439));
#4983=DIRECTION('',(-0.5,0.,0.866025403784439));
#4984=DIRECTION('',(0.,-1.,0.));
#4985=DIRECTION('',(0.5,0.,-0.866025403784439));
#4986=DIRECTION('center_axis',(-0.866025403784439,0.,0.5));
#4987=DIRECTION('ref_axis',(-0.5,0.,-0.866025403784439));
#4988=DIRECTION('',(0.5,0.,0.866025403784439));
#4989=DIRECTION('',(0.,-1.,0.));
#4990=DIRECTION('',(-0.5,0.,-0.866025403784439));
#4991=DIRECTION('center_axis',(-2.40370335797945E-16,0.,1.));
#4992=DIRECTION('ref_axis',(-1.,0.,-2.40370335797945E-16));
#4993=DIRECTION('',(1.,0.,2.40370335797945E-16));
#4994=DIRECTION('',(0.,-1.,0.));
#4995=DIRECTION('',(-1.,0.,-2.40370335797945E-16));
#4996=DIRECTION('center_axis',(0.866025403784439,0.,0.5));
#4997=DIRECTION('ref_axis',(-0.5,0.,0.866025403784439));
#4998=DIRECTION('',(0.5,0.,-0.866025403784439));
#4999=DIRECTION('',(-0.5,0.,0.866025403784439));
#5000=DIRECTION('center_axis',(0.,1.,0.));
#5001=DIRECTION('ref_axis',(1.,0.,0.));
#5002=DIRECTION('center_axis',(0.,-1.,0.));
#5003=DIRECTION('ref_axis',(0.,0.,-1.));
#5004=DIRECTION('center_axis',(0.,1.,0.));
#5005=DIRECTION('ref_axis',(1.,0.,0.));
#5006=DIRECTION('center_axis',(0.,1.,0.));
#5007=DIRECTION('ref_axis',(1.,0.,0.));
#5008=DIRECTION('center_axis',(0.,1.,0.));
#5009=DIRECTION('ref_axis',(0.,0.,1.));
#5010=DIRECTION('center_axis',(0.,-1.,0.));
#5011=DIRECTION('ref_axis',(1.,0.,0.));
#5012=DIRECTION('center_axis',(0.,-1.,0.));
#5013=DIRECTION('ref_axis',(1.,0.,0.));
#5014=DIRECTION('center_axis',(0.,-1.,0.));
#5015=DIRECTION('ref_axis',(1.,0.,0.));
#5016=DIRECTION('',(0.707106781186548,0.707106781186547,8.65956056235493E-17));
#5017=DIRECTION('center_axis',(0.,-1.,0.));
#5018=DIRECTION('ref_axis',(1.,0.,0.));
#5019=DIRECTION('center_axis',(0.,-1.,0.));
#5020=DIRECTION('ref_axis',(1.,0.,0.));
#5021=DIRECTION('',(0.,1.,0.));
#5022=DIRECTION('center_axis',(0.,1.,0.));
#5023=DIRECTION('ref_axis',(1.,0.,0.));
#5024=DIRECTION('center_axis',(0.,-1.,0.));
#5025=DIRECTION('ref_axis',(1.,0.,0.));
#5026=DIRECTION('',(-0.707106781186547,0.707106781186548,-8.65956056235493E-17));
#5027=DIRECTION('center_axis',(0.,-1.,0.));
#5028=DIRECTION('ref_axis',(0.,0.,-1.));
#5029=DIRECTION('center_axis',(0.,-1.,0.));
#5030=DIRECTION('ref_axis',(1.,0.,0.));
#5031=DIRECTION('center_axis',(0.,1.,0.));
#5032=DIRECTION('ref_axis',(1.,0.,0.));
#5033=DIRECTION('center_axis',(0.,1.,0.));
#5034=DIRECTION('ref_axis',(1.,0.,0.));
#5035=DIRECTION('',(-0.447213595499958,0.894427190999916,-5.47678698264203E-17));
#5036=DIRECTION('center_axis',(0.,-1.,0.));
#5037=DIRECTION('ref_axis',(1.,0.,0.));
#5038=DIRECTION('',(0.,1.,0.));
#5039=DIRECTION('axis',(0.,0.,1.));
#5040=DIRECTION('refdir',(1.,0.,0.));
#5041=DIRECTION('center_axis',(0.866025403784439,0.,-0.5));
#5042=DIRECTION('ref_axis',(0.5,0.,0.866025403784439));
#5043=DIRECTION('',(-0.5,0.,-0.866025403784439));
#5044=DIRECTION('',(0.,-1.,0.));
#5045=DIRECTION('',(0.5,0.,0.866025403784439));
#5046=DIRECTION('',(0.,-1.,0.));
#5047=DIRECTION('center_axis',(1.60246890531964E-16,0.,-1.));
#5048=DIRECTION('ref_axis',(1.,0.,1.60246890531964E-16));
#5049=DIRECTION('',(-1.,0.,-1.60246890531964E-16));
#5050=DIRECTION('',(0.,-1.,0.));
#5051=DIRECTION('',(1.,0.,1.60246890531964E-16));
#5052=DIRECTION('center_axis',(-0.866025403784439,0.,-0.5));
#5053=DIRECTION('ref_axis',(0.5,0.,-0.866025403784439));
#5054=DIRECTION('',(-0.5,0.,0.866025403784439));
#5055=DIRECTION('',(0.,-1.,0.));
#5056=DIRECTION('',(0.5,0.,-0.866025403784439));
#5057=DIRECTION('center_axis',(-0.866025403784439,0.,0.5));
#5058=DIRECTION('ref_axis',(-0.5,0.,-0.866025403784439));
#5059=DIRECTION('',(0.5,0.,0.866025403784439));
#5060=DIRECTION('',(0.,-1.,0.));
#5061=DIRECTION('',(-0.5,0.,-0.866025403784439));
#5062=DIRECTION('center_axis',(-1.60246890531964E-16,0.,1.));
#5063=DIRECTION('ref_axis',(-1.,0.,-1.60246890531964E-16));
#5064=DIRECTION('',(1.,0.,1.60246890531964E-16));
#5065=DIRECTION('',(0.,-1.,0.));
#5066=DIRECTION('',(-1.,0.,-1.60246890531964E-16));
#5067=DIRECTION('center_axis',(0.866025403784439,0.,0.5));
#5068=DIRECTION('ref_axis',(-0.5,0.,0.866025403784439));
#5069=DIRECTION('',(0.5,0.,-0.866025403784439));
#5070=DIRECTION('',(-0.5,0.,0.866025403784439));
#5071=DIRECTION('center_axis',(0.,1.,0.));
#5072=DIRECTION('ref_axis',(1.,0.,0.));
#5073=DIRECTION('center_axis',(0.,-1.,0.));
#5074=DIRECTION('ref_axis',(0.,0.,-1.));
#5075=DIRECTION('center_axis',(0.,1.,0.));
#5076=DIRECTION('ref_axis',(1.,0.,0.));
#5077=DIRECTION('center_axis',(0.,1.,0.));
#5078=DIRECTION('ref_axis',(1.,0.,0.));
#5079=DIRECTION('center_axis',(0.,1.,0.));
#5080=DIRECTION('ref_axis',(0.,0.,1.));
#5081=DIRECTION('center_axis',(0.,-1.,0.));
#5082=DIRECTION('ref_axis',(1.,0.,0.));
#5083=DIRECTION('center_axis',(0.,-1.,0.));
#5084=DIRECTION('ref_axis',(1.,0.,0.));
#5085=DIRECTION('center_axis',(0.,-1.,0.));
#5086=DIRECTION('ref_axis',(1.,0.,0.));
#5087=DIRECTION('',(0.707106781186547,0.707106781186548,8.65956056235493E-17));
#5088=DIRECTION('center_axis',(0.,-1.,0.));
#5089=DIRECTION('ref_axis',(1.,0.,0.));
#5090=DIRECTION('center_axis',(0.,-1.,0.));
#5091=DIRECTION('ref_axis',(1.,0.,0.));
#5092=DIRECTION('',(0.,1.,0.));
#5093=DIRECTION('center_axis',(0.,1.,0.));
#5094=DIRECTION('ref_axis',(1.,0.,0.));
#5095=DIRECTION('center_axis',(0.,-1.,0.));
#5096=DIRECTION('ref_axis',(1.,0.,0.));
#5097=DIRECTION('',(-0.707106781186547,0.707106781186548,-8.65956056235493E-17));
#5098=DIRECTION('center_axis',(0.,-1.,0.));
#5099=DIRECTION('ref_axis',(0.,0.,-1.));
#5100=DIRECTION('center_axis',(0.,-1.,0.));
#5101=DIRECTION('ref_axis',(1.,0.,0.));
#5102=DIRECTION('center_axis',(0.,1.,0.));
#5103=DIRECTION('ref_axis',(1.,0.,0.));
#5104=DIRECTION('center_axis',(0.,1.,0.));
#5105=DIRECTION('ref_axis',(1.,0.,0.));
#5106=DIRECTION('',(-0.447213595499958,0.894427190999916,-5.47678698264203E-17));
#5107=DIRECTION('center_axis',(0.,-1.,0.));
#5108=DIRECTION('ref_axis',(1.,0.,0.));
#5109=DIRECTION('',(0.,1.,0.));
#5110=DIRECTION('',(0.,0.,1.));
#5111=DIRECTION('',(1.,0.,0.));
#5112=DIRECTION('',(0.,0.,1.));
#5113=DIRECTION('',(1.,0.,0.));
#5114=DIRECTION('',(0.,0.,1.));
#5115=DIRECTION('',(1.,0.,0.));
#5116=DIRECTION('',(0.,0.,1.));
#5117=DIRECTION('',(1.,0.,0.));
#5118=DIRECTION('',(0.,0.,1.));
#5119=DIRECTION('',(1.,0.,0.));
#5120=DIRECTION('',(0.,0.,1.));
#5121=DIRECTION('',(1.,0.,0.));
#5122=DIRECTION('',(0.,0.,1.));
#5123=DIRECTION('',(1.,0.,0.));
#5124=DIRECTION('',(0.,0.,1.));
#5125=DIRECTION('',(1.,0.,0.));
#5126=DIRECTION('',(0.,0.,1.));
#5127=DIRECTION('',(1.,0.,0.));
#5128=DIRECTION('',(0.,0.,1.));
#5129=DIRECTION('',(1.,0.,0.));
#5130=DIRECTION('',(0.,0.,1.));
#5131=DIRECTION('',(1.,0.,0.));
#5132=DIRECTION('',(0.,0.,1.));
#5133=DIRECTION('',(1.,0.,0.));
#5134=DIRECTION('',(0.,0.,1.));
#5135=DIRECTION('',(1.,0.,0.));
#5136=DIRECTION('',(0.,0.,1.));
#5137=DIRECTION('',(1.,0.,0.));
#5138=DIRECTION('',(0.,0.,1.));
#5139=DIRECTION('',(1.,0.,0.));
#5140=DIRECTION('',(0.,-1.,2.22044604925031E-16));
#5141=DIRECTION('',(1.,0.,0.));
#5142=DIRECTION('',(0.,-1.,2.22044604925031E-16));
#5143=DIRECTION('',(1.,0.,0.));
#5144=DIRECTION('',(0.,-1.,2.22044604925031E-16));
#5145=DIRECTION('',(1.,0.,0.));
#5146=DIRECTION('',(0.,-1.,2.22044604925031E-16));
#5147=DIRECTION('',(1.,0.,0.));
#5148=DIRECTION('',(0.,-1.,2.22044604925031E-16));
#5149=DIRECTION('',(1.,0.,0.));
#5150=DIRECTION('',(0.,-1.,2.22044604925031E-16));
#5151=DIRECTION('',(1.,0.,0.));
#5152=DIRECTION('',(0.,-1.,2.22044604925031E-16));
#5153=DIRECTION('',(1.,0.,0.));
#5154=DIRECTION('',(0.,-1.,2.22044604925031E-16));
#5155=DIRECTION('',(1.,0.,0.));
#5156=DIRECTION('',(0.,0.,1.));
#5157=DIRECTION('',(2.22044604925031E-16,1.,0.));
#5158=DIRECTION('',(0.,0.,1.));
#5159=DIRECTION('',(2.22044604925031E-16,-1.,0.));
#5160=DIRECTION('',(0.,-1.,2.22044604925031E-16));
#5161=DIRECTION('',(1.,0.,0.));
#5162=DIRECTION('',(0.,-1.,2.22044604925031E-16));
#5163=DIRECTION('',(1.,0.,0.));
#5164=DIRECTION('',(0.,-1.,2.22044604925031E-16));
#5165=DIRECTION('',(1.,0.,0.));
#5166=DIRECTION('axis',(0.,0.,1.));
#5167=DIRECTION('refdir',(1.,0.,0.));
#5168=DIRECTION('axis',(0.,0.,1.));
#5169=DIRECTION('refdir',(1.,0.,0.));
#5170=DIRECTION('center_axis',(0.,0.,1.));
#5171=DIRECTION('ref_axis',(1.,0.,0.));
#5172=DIRECTION('center_axis',(0.,0.,1.));
#5173=DIRECTION('ref_axis',(1.,0.,0.));
#5174=DIRECTION('',(0.,0.,1.));
#5175=DIRECTION('center_axis',(0.,0.,-1.));
#5176=DIRECTION('ref_axis',(1.,0.,0.));
#5177=DIRECTION('center_axis',(0.,0.,1.));
#5178=DIRECTION('ref_axis',(1.,0.,0.));
#5179=DIRECTION('center_axis',(0.,0.,1.));
#5180=DIRECTION('ref_axis',(1.,0.,0.));
#5181=DIRECTION('',(0.,0.,1.));
#5182=DIRECTION('center_axis',(0.,0.,-1.));
#5183=DIRECTION('ref_axis',(1.,0.,0.));
#5184=DIRECTION('center_axis',(0.,0.,1.));
#5185=DIRECTION('ref_axis',(1.,0.,0.));
#5186=DIRECTION('center_axis',(0.,0.,1.));
#5187=DIRECTION('ref_axis',(1.,0.,0.));
#5188=DIRECTION('',(0.,0.,1.));
#5189=DIRECTION('center_axis',(0.,0.,-1.));
#5190=DIRECTION('ref_axis',(1.,0.,0.));
#5191=DIRECTION('center_axis',(0.,0.,1.));
#5192=DIRECTION('ref_axis',(1.,0.,0.));
#5193=DIRECTION('center_axis',(0.,0.,1.));
#5194=DIRECTION('ref_axis',(1.,0.,0.));
#5195=DIRECTION('',(0.,0.,1.));
#5196=DIRECTION('center_axis',(0.,0.,-1.));
#5197=DIRECTION('ref_axis',(1.,0.,0.));
#5198=DIRECTION('center_axis',(1.,0.,0.));
#5199=DIRECTION('ref_axis',(0.,0.,-1.));
#5200=DIRECTION('center_axis',(1.,0.,0.));
#5201=DIRECTION('ref_axis',(0.,0.,-1.));
#5202=DIRECTION('',(0.,-1.,0.));
#5203=DIRECTION('',(0.,0.,1.));
#5204=DIRECTION('',(0.,1.,0.));
#5205=DIRECTION('center_axis',(-1.,0.,0.));
#5206=DIRECTION('ref_axis',(0.,0.,-1.));
#5207=DIRECTION('center_axis',(0.,0.,1.));
#5208=DIRECTION('ref_axis',(0.,-1.,0.));
#5209=DIRECTION('',(1.,0.,0.));
#5210=DIRECTION('',(1.,0.,0.));
#5211=DIRECTION('',(0.,-1.,0.));
#5212=DIRECTION('center_axis',(1.,0.,0.));
#5213=DIRECTION('ref_axis',(0.,0.,-1.));
#5214=DIRECTION('center_axis',(1.,0.,0.));
#5215=DIRECTION('ref_axis',(0.,0.,-1.));
#5216=DIRECTION('',(0.,1.,0.));
#5217=DIRECTION('',(0.,0.,-1.));
#5218=DIRECTION('center_axis',(-1.,0.,0.));
#5219=DIRECTION('ref_axis',(0.,0.,-1.));
#5220=DIRECTION('center_axis',(1.,0.,0.));
#5221=DIRECTION('ref_axis',(0.,0.,-1.));
#5222=DIRECTION('',(-1.,0.,0.));
#5223=DIRECTION('center_axis',(1.,0.,0.));
#5224=DIRECTION('ref_axis',(0.,0.,-1.));
#5225=DIRECTION('',(1.,0.,0.));
#5226=DIRECTION('center_axis',(0.,-1.,0.));
#5227=DIRECTION('ref_axis',(1.,0.,0.));
#5228=DIRECTION('',(1.,0.,0.));
#5229=DIRECTION('',(0.,0.,1.));
#5230=DIRECTION('',(1.,0.,0.));
#5231=DIRECTION('',(0.,0.,-1.));
#5232=DIRECTION('',(1.,0.,0.));
#5233=DIRECTION('center_axis',(-1.,0.,0.));
#5234=DIRECTION('ref_axis',(0.,-1.,0.));
#5235=DIRECTION('',(0.,-1.,0.));
#5236=DIRECTION('',(0.,0.,1.));
#5237=DIRECTION('',(0.,1.,0.));
#5238=DIRECTION('center_axis',(0.,1.,0.));
#5239=DIRECTION('ref_axis',(-1.,0.,0.));
#5240=DIRECTION('',(-1.,0.,0.));
#5241=DIRECTION('',(0.,0.,1.));
#5242=DIRECTION('',(1.,0.,0.));
#5243=DIRECTION('center_axis',(1.,0.,0.));
#5244=DIRECTION('ref_axis',(0.,1.,0.));
#5245=DIRECTION('',(0.,1.,0.));
#5246=DIRECTION('',(0.,0.,-1.));
#5247=DIRECTION('',(0.,-1.,0.));
#5248=DIRECTION('center_axis',(0.,0.,1.));
#5249=DIRECTION('ref_axis',(1.,0.,0.));
#5250=DIRECTION('',(0.,1.,0.));
#5251=DIRECTION('',(-1.,0.,0.));
#5252=DIRECTION('',(0.,-1.,0.));
#5253=DIRECTION('',(1.,0.,0.));
#5254=DIRECTION('',(0.,-1.,0.));
#5255=DIRECTION('',(-1.,0.,0.));
#5256=DIRECTION('',(0.,1.,0.));
#5257=DIRECTION('',(1.,0.,0.));
#5258=DIRECTION('center_axis',(1.,0.,0.));
#5259=DIRECTION('ref_axis',(0.,1.,0.));
#5260=DIRECTION('',(0.,-1.,0.));
#5261=DIRECTION('',(0.,0.,1.));
#5262=DIRECTION('center_axis',(0.,1.,0.));
#5263=DIRECTION('ref_axis',(-1.,0.,0.));
#5264=DIRECTION('',(1.,0.,0.));
#5265=DIRECTION('',(0.,0.,1.));
#5266=DIRECTION('center_axis',(-1.,0.,0.));
#5267=DIRECTION('ref_axis',(0.,-1.,0.));
#5268=DIRECTION('',(0.,1.,0.));
#5269=DIRECTION('',(0.,0.,1.));
#5270=DIRECTION('center_axis',(0.,-1.,0.));
#5271=DIRECTION('ref_axis',(1.,0.,0.));
#5272=DIRECTION('',(1.,0.,0.));
#5273=DIRECTION('',(0.,0.,1.));
#5274=DIRECTION('center_axis',(0.,-1.,0.));
#5275=DIRECTION('ref_axis',(1.,0.,0.));
#5276=DIRECTION('',(0.,0.,1.));
#5277=DIRECTION('',(1.,0.,0.));
#5278=DIRECTION('center_axis',(0.,1.,0.));
#5279=DIRECTION('ref_axis',(-1.,0.,0.));
#5280=DIRECTION('',(0.,0.,1.));
#5281=DIRECTION('',(-1.,0.,0.));
#5282=DIRECTION('',(0.,0.,1.));
#5283=DIRECTION('center_axis',(1.,0.,0.));
#5284=DIRECTION('ref_axis',(0.,1.,0.));
#5285=DIRECTION('',(0.,1.,0.));
#5286=DIRECTION('center_axis',(-1.,0.,0.));
#5287=DIRECTION('ref_axis',(0.,-1.,0.));
#5288=DIRECTION('',(0.,-1.,0.));
#5289=DIRECTION('center_axis',(0.,0.,1.));
#5290=DIRECTION('ref_axis',(1.,0.,0.));
#5291=DIRECTION('axis',(0.,0.,1.));
#5292=DIRECTION('refdir',(1.,0.,0.));
#5293=DIRECTION('center_axis',(0.,0.,1.));
#5294=DIRECTION('ref_axis',(1.,0.,0.));
#5295=DIRECTION('center_axis',(0.,0.,1.));
#5296=DIRECTION('ref_axis',(1.,0.,0.));
#5297=DIRECTION('center_axis',(0.,0.,1.));
#5298=DIRECTION('ref_axis',(1.,0.,0.));
#5299=DIRECTION('center_axis',(0.,0.,1.));
#5300=DIRECTION('ref_axis',(1.,0.,0.));
#5301=DIRECTION('center_axis',(0.,0.,1.));
#5302=DIRECTION('ref_axis',(1.,0.,0.));
#5303=DIRECTION('',(0.,0.,-1.));
#5304=DIRECTION('center_axis',(0.,0.,1.));
#5305=DIRECTION('ref_axis',(1.,0.,0.));
#5306=DIRECTION('center_axis',(0.,0.,-1.));
#5307=DIRECTION('ref_axis',(1.,0.,0.));
#5308=DIRECTION('center_axis',(0.,0.,1.));
#5309=DIRECTION('ref_axis',(1.,0.,0.));
#5310=DIRECTION('',(0.,0.,-1.));
#5311=DIRECTION('center_axis',(0.,0.,-1.));
#5312=DIRECTION('ref_axis',(1.,0.,0.));
#5313=DIRECTION('center_axis',(0.,0.,1.));
#5314=DIRECTION('ref_axis',(1.,0.,0.));
#5315=DIRECTION('',(0.,0.,-1.));
#5316=DIRECTION('center_axis',(0.,0.,1.));
#5317=DIRECTION('ref_axis',(1.,0.,0.));
#5318=DIRECTION('center_axis',(0.,0.,1.));
#5319=DIRECTION('ref_axis',(1.,0.,0.));
#5320=DIRECTION('axis',(0.,0.,1.));
#5321=DIRECTION('refdir',(1.,0.,0.));
#5322=DIRECTION('center_axis',(0.,0.,1.));
#5323=DIRECTION('ref_axis',(1.,0.,0.));
#5324=DIRECTION('center_axis',(0.,0.,1.));
#5325=DIRECTION('ref_axis',(1.,0.,0.));
#5326=DIRECTION('center_axis',(0.,0.,1.));
#5327=DIRECTION('ref_axis',(1.,0.,0.));
#5328=DIRECTION('center_axis',(0.,0.,1.));
#5329=DIRECTION('ref_axis',(1.,0.,0.));
#5330=DIRECTION('center_axis',(0.,0.,1.));
#5331=DIRECTION('ref_axis',(1.,0.,0.));
#5332=DIRECTION('',(0.,0.,-1.));
#5333=DIRECTION('center_axis',(0.,0.,1.));
#5334=DIRECTION('ref_axis',(1.,0.,0.));
#5335=DIRECTION('center_axis',(0.,0.,-1.));
#5336=DIRECTION('ref_axis',(1.,0.,0.));
#5337=DIRECTION('center_axis',(0.,0.,1.));
#5338=DIRECTION('ref_axis',(1.,0.,0.));
#5339=DIRECTION('',(0.,0.,-1.));
#5340=DIRECTION('center_axis',(0.,0.,-1.));
#5341=DIRECTION('ref_axis',(1.,0.,0.));
#5342=DIRECTION('center_axis',(0.,0.,1.));
#5343=DIRECTION('ref_axis',(1.,0.,0.));
#5344=DIRECTION('',(0.,0.,-1.));
#5345=DIRECTION('center_axis',(0.,0.,1.));
#5346=DIRECTION('ref_axis',(1.,0.,0.));
#5347=DIRECTION('center_axis',(0.,0.,1.));
#5348=DIRECTION('ref_axis',(1.,0.,0.));
#5349=DIRECTION('axis',(0.,0.,1.));
#5350=DIRECTION('refdir',(1.,0.,0.));
#5351=DIRECTION('center_axis',(0.,0.,1.));
#5352=DIRECTION('ref_axis',(1.,0.,0.));
#5353=DIRECTION('center_axis',(0.,0.,1.));
#5354=DIRECTION('ref_axis',(1.,0.,0.));
#5355=DIRECTION('center_axis',(0.,0.,1.));
#5356=DIRECTION('ref_axis',(1.,0.,0.));
#5357=DIRECTION('center_axis',(0.,0.,1.));
#5358=DIRECTION('ref_axis',(1.,0.,0.));
#5359=DIRECTION('center_axis',(0.,0.,1.));
#5360=DIRECTION('ref_axis',(1.,0.,0.));
#5361=DIRECTION('',(0.,0.,-1.));
#5362=DIRECTION('center_axis',(0.,0.,1.));
#5363=DIRECTION('ref_axis',(1.,0.,0.));
#5364=DIRECTION('center_axis',(0.,0.,-1.));
#5365=DIRECTION('ref_axis',(1.,0.,0.));
#5366=DIRECTION('center_axis',(0.,0.,1.));
#5367=DIRECTION('ref_axis',(1.,0.,0.));
#5368=DIRECTION('',(0.,0.,-1.));
#5369=DIRECTION('center_axis',(0.,0.,-1.));
#5370=DIRECTION('ref_axis',(1.,0.,0.));
#5371=DIRECTION('center_axis',(0.,0.,1.));
#5372=DIRECTION('ref_axis',(1.,0.,0.));
#5373=DIRECTION('',(0.,0.,-1.));
#5374=DIRECTION('center_axis',(0.,0.,1.));
#5375=DIRECTION('ref_axis',(1.,0.,0.));
#5376=DIRECTION('center_axis',(0.,0.,1.));
#5377=DIRECTION('ref_axis',(1.,0.,0.));
#5378=DIRECTION('axis',(0.,0.,1.));
#5379=DIRECTION('refdir',(1.,0.,0.));
#5380=DIRECTION('center_axis',(0.,0.,1.));
#5381=DIRECTION('ref_axis',(1.,0.,0.));
#5382=DIRECTION('center_axis',(0.,0.,1.));
#5383=DIRECTION('ref_axis',(1.,0.,0.));
#5384=DIRECTION('center_axis',(0.,0.,1.));
#5385=DIRECTION('ref_axis',(1.,0.,0.));
#5386=DIRECTION('center_axis',(0.,0.,1.));
#5387=DIRECTION('ref_axis',(1.,0.,0.));
#5388=DIRECTION('center_axis',(0.,0.,1.));
#5389=DIRECTION('ref_axis',(1.,0.,0.));
#5390=DIRECTION('',(0.,0.,-1.));
#5391=DIRECTION('center_axis',(0.,0.,1.));
#5392=DIRECTION('ref_axis',(1.,0.,0.));
#5393=DIRECTION('center_axis',(0.,0.,-1.));
#5394=DIRECTION('ref_axis',(1.,0.,0.));
#5395=DIRECTION('center_axis',(0.,0.,1.));
#5396=DIRECTION('ref_axis',(1.,0.,0.));
#5397=DIRECTION('',(0.,0.,-1.));
#5398=DIRECTION('center_axis',(0.,0.,-1.));
#5399=DIRECTION('ref_axis',(1.,0.,0.));
#5400=DIRECTION('center_axis',(0.,0.,1.));
#5401=DIRECTION('ref_axis',(1.,0.,0.));
#5402=DIRECTION('',(0.,0.,-1.));
#5403=DIRECTION('center_axis',(0.,0.,1.));
#5404=DIRECTION('ref_axis',(1.,0.,0.));
#5405=DIRECTION('center_axis',(0.,0.,1.));
#5406=DIRECTION('ref_axis',(1.,0.,0.));
#5407=DIRECTION('',(0.,0.,1.));
#5408=DIRECTION('',(1.,0.,0.));
#5409=DIRECTION('',(0.,0.,1.));
#5410=DIRECTION('',(1.,0.,0.));
#5411=DIRECTION('',(0.,0.,1.));
#5412=DIRECTION('',(1.,0.,0.));
#5413=DIRECTION('',(0.,0.,1.));
#5414=DIRECTION('',(1.,0.,0.));
#5415=DIRECTION('',(0.,0.,1.));
#5416=DIRECTION('',(1.,0.,0.));
#5417=DIRECTION('axis',(0.,0.,1.));
#5418=DIRECTION('refdir',(1.,0.,0.));
#5419=DIRECTION('axis',(0.,0.,1.));
#5420=DIRECTION('refdir',(1.,0.,0.));
#5421=DIRECTION('center_axis',(0.,0.,1.));
#5422=DIRECTION('ref_axis',(1.,0.,0.));
#5423=DIRECTION('center_axis',(0.,0.,1.));
#5424=DIRECTION('ref_axis',(1.,0.,0.));
#5425=DIRECTION('',(0.,0.,1.));
#5426=DIRECTION('center_axis',(0.,0.,-1.));
#5427=DIRECTION('ref_axis',(1.,0.,0.));
#5428=DIRECTION('center_axis',(1.,0.,0.));
#5429=DIRECTION('ref_axis',(0.,1.,0.));
#5430=DIRECTION('',(0.,0.,1.));
#5431=DIRECTION('',(0.,1.,0.));
#5432=DIRECTION('',(0.,0.,1.));
#5433=DIRECTION('',(0.,1.,0.));
#5434=DIRECTION('center_axis',(0.,1.,0.));
#5435=DIRECTION('ref_axis',(-1.,0.,0.));
#5436=DIRECTION('',(-1.,0.,0.));
#5437=DIRECTION('',(0.,0.,1.));
#5438=DIRECTION('',(-1.,0.,0.));
#5439=DIRECTION('center_axis',(-1.,0.,0.));
#5440=DIRECTION('ref_axis',(0.,-1.,0.));
#5441=DIRECTION('',(0.,0.,-1.));
#5442=DIRECTION('',(0.,-1.,0.));
#5443=DIRECTION('',(0.,-1.,0.));
#5444=DIRECTION('center_axis',(0.,0.,1.));
#5445=DIRECTION('ref_axis',(1.,0.,0.));
#5446=DIRECTION('center_axis',(0.,0.,1.));
#5447=DIRECTION('ref_axis',(1.,0.,0.));
#5448=DIRECTION('center_axis',(0.,0.,1.));
#5449=DIRECTION('ref_axis',(1.,0.,0.));
#5450=DIRECTION('center_axis',(0.,0.,1.));
#5451=DIRECTION('ref_axis',(1.,0.,0.));
#5452=DIRECTION('center_axis',(0.,0.,1.));
#5453=DIRECTION('ref_axis',(1.,0.,0.));
#5454=DIRECTION('center_axis',(0.,0.,1.));
#5455=DIRECTION('ref_axis',(-0.149222317351604,-0.988803671111823,0.));
#5456=DIRECTION('center_axis',(0.,0.,1.));
#5457=DIRECTION('ref_axis',(1.,0.,0.));
#5458=DIRECTION('',(0.,0.,-1.));
#5459=DIRECTION('center_axis',(0.,0.,1.));
#5460=DIRECTION('ref_axis',(1.,0.,0.));
#5461=DIRECTION('center_axis',(0.,0.,1.));
#5462=DIRECTION('ref_axis',(1.,0.,0.));
#5463=DIRECTION('axis',(0.,0.,1.));
#5464=DIRECTION('refdir',(1.,0.,0.));
#5465=DIRECTION('center_axis',(0.,0.,1.));
#5466=DIRECTION('ref_axis',(1.,0.,0.));
#5467=DIRECTION('center_axis',(0.,0.,1.));
#5468=DIRECTION('ref_axis',(1.,0.,0.));
#5469=DIRECTION('',(0.,0.,-1.));
#5470=DIRECTION('center_axis',(0.,0.,1.));
#5471=DIRECTION('ref_axis',(1.,0.,0.));
#5472=DIRECTION('center_axis',(0.,0.,1.));
#5473=DIRECTION('ref_axis',(1.,0.,0.));
#5474=DIRECTION('center_axis',(0.,0.,1.));
#5475=DIRECTION('ref_axis',(1.,0.,0.));
#5476=DIRECTION('',(0.,0.,1.));
#5477=DIRECTION('',(1.,0.,0.));
#5478=DIRECTION('',(0.,0.,1.));
#5479=DIRECTION('',(1.,0.,0.));
#5480=DIRECTION('',(0.,0.,1.));
#5481=DIRECTION('',(1.,0.,0.));
#5482=DIRECTION('',(0.,0.,1.));
#5483=DIRECTION('',(1.,0.,0.));
#5484=DIRECTION('',(0.,0.,1.));
#5485=DIRECTION('',(1.,0.,0.));
#5486=CARTESIAN_POINT('',(0.,0.,0.));
#5487=CARTESIAN_POINT('',(0.,0.,0.));
#5488=CARTESIAN_POINT('',(0.,0.,0.));
#5489=CARTESIAN_POINT('Origin',(9.2,2.7,-0.1));
#5490=CARTESIAN_POINT('',(9.035,2.7,0.));
#5491=CARTESIAN_POINT('Origin',(9.2,2.7,0.));
#5492=CARTESIAN_POINT('',(9.035,2.7,1.));
#5493=CARTESIAN_POINT('',(9.035,2.7,-0.1));
#5494=CARTESIAN_POINT('Origin',(9.2,2.7,1.));
#5495=CARTESIAN_POINT('Origin',(9.2,4.3,-0.1));
#5496=CARTESIAN_POINT('',(9.035,4.3,0.));
#5497=CARTESIAN_POINT('Origin',(9.2,4.3,0.));
#5498=CARTESIAN_POINT('',(9.035,4.3,1.));
#5499=CARTESIAN_POINT('',(9.035,4.3,-0.1));
#5500=CARTESIAN_POINT('Origin',(9.2,4.3,1.));
#5501=CARTESIAN_POINT('Origin',(3.5,-1.8,-0.1));
#5502=CARTESIAN_POINT('',(3.29,-1.8,0.));
#5503=CARTESIAN_POINT('Origin',(3.5,-1.8,0.));
#5504=CARTESIAN_POINT('',(3.29,-1.8,1.));
#5505=CARTESIAN_POINT('',(3.29,-1.8,-0.1));
#5506=CARTESIAN_POINT('Origin',(3.5,-1.8,1.));
#5507=CARTESIAN_POINT('Origin',(-3.5,1.8,-0.1));
#5508=CARTESIAN_POINT('',(-3.71,1.8,0.));
#5509=CARTESIAN_POINT('Origin',(-3.5,1.8,0.));
#5510=CARTESIAN_POINT('',(-3.71,1.8,1.));
#5511=CARTESIAN_POINT('',(-3.71,1.8,-0.1));
#5512=CARTESIAN_POINT('Origin',(-3.5,1.8,1.));
#5513=CARTESIAN_POINT('Origin',(-3.5,-1.8,-0.1));
#5514=CARTESIAN_POINT('',(-3.71,-1.8,0.));
#5515=CARTESIAN_POINT('Origin',(-3.5,-1.8,0.));
#5516=CARTESIAN_POINT('',(-3.71,-1.8,1.));
#5517=CARTESIAN_POINT('',(-3.71,-1.8,-0.1));
#5518=CARTESIAN_POINT('Origin',(-3.5,-1.8,1.));
#5519=CARTESIAN_POINT('Origin',(3.5,1.8,-0.1));
#5520=CARTESIAN_POINT('',(3.29,1.8,0.));
#5521=CARTESIAN_POINT('Origin',(3.5,1.8,0.));
#5522=CARTESIAN_POINT('',(3.29,1.8,1.));
#5523=CARTESIAN_POINT('',(3.29,1.8,-0.1));
#5524=CARTESIAN_POINT('Origin',(3.5,1.8,1.));
#5525=CARTESIAN_POINT('Origin',(3.,-1.8,-0.1));
#5526=CARTESIAN_POINT('',(2.79,-1.8,0.));
#5527=CARTESIAN_POINT('Origin',(3.,-1.8,0.));
#5528=CARTESIAN_POINT('',(2.79,-1.8,1.));
#5529=CARTESIAN_POINT('',(2.79,-1.8,-0.1));
#5530=CARTESIAN_POINT('Origin',(3.,-1.8,1.));
#5531=CARTESIAN_POINT('Origin',(-3.,1.8,-0.1));
#5532=CARTESIAN_POINT('',(-3.21,1.8,0.));
#5533=CARTESIAN_POINT('Origin',(-3.,1.8,0.));
#5534=CARTESIAN_POINT('',(-3.21,1.8,1.));
#5535=CARTESIAN_POINT('',(-3.21,1.8,-0.1));
#5536=CARTESIAN_POINT('Origin',(-3.,1.8,1.));
#5537=CARTESIAN_POINT('Origin',(-3.,-1.8,-0.1));
#5538=CARTESIAN_POINT('',(-3.21,-1.8,0.));
#5539=CARTESIAN_POINT('Origin',(-3.,-1.8,0.));
#5540=CARTESIAN_POINT('',(-3.21,-1.8,1.));
#5541=CARTESIAN_POINT('',(-3.21,-1.8,-0.1));
#5542=CARTESIAN_POINT('Origin',(-3.,-1.8,1.));
#5543=CARTESIAN_POINT('Origin',(3.,1.8,-0.1));
#5544=CARTESIAN_POINT('',(2.79,1.8,0.));
#5545=CARTESIAN_POINT('Origin',(3.,1.8,0.));
#5546=CARTESIAN_POINT('',(2.79,1.8,1.));
#5547=CARTESIAN_POINT('',(2.79,1.8,-0.1));
#5548=CARTESIAN_POINT('Origin',(3.,1.8,1.));
#5549=CARTESIAN_POINT('Origin',(6.5,-6.5,-0.1));
#5550=CARTESIAN_POINT('',(6.29,-6.5,0.));
#5551=CARTESIAN_POINT('Origin',(6.5,-6.5,0.));
#5552=CARTESIAN_POINT('',(6.29,-6.5,1.));
#5553=CARTESIAN_POINT('',(6.29,-6.5,-0.1));
#5554=CARTESIAN_POINT('Origin',(6.5,-6.5,1.));
#5555=CARTESIAN_POINT('Origin',(-6.5,-4.2,-0.1));
#5556=CARTESIAN_POINT('',(-6.71,-4.2,0.));
#5557=CARTESIAN_POINT('Origin',(-6.5,-4.2,0.));
#5558=CARTESIAN_POINT('',(-6.71,-4.2,1.));
#5559=CARTESIAN_POINT('',(-6.71,-4.2,-0.1));
#5560=CARTESIAN_POINT('Origin',(-6.5,-4.2,1.));
#5561=CARTESIAN_POINT('Origin',(-6.5,-6.5,-0.1));
#5562=CARTESIAN_POINT('',(-6.71,-6.5,0.));
#5563=CARTESIAN_POINT('Origin',(-6.5,-6.5,0.));
#5564=CARTESIAN_POINT('',(-6.71,-6.5,1.));
#5565=CARTESIAN_POINT('',(-6.71,-6.5,-0.1));
#5566=CARTESIAN_POINT('Origin',(-6.5,-6.5,1.));
#5567=CARTESIAN_POINT('Origin',(6.5,-4.2,-0.1));
#5568=CARTESIAN_POINT('',(6.29,-4.2,0.));
#5569=CARTESIAN_POINT('Origin',(6.5,-4.2,0.));
#5570=CARTESIAN_POINT('',(6.29,-4.2,1.));
#5571=CARTESIAN_POINT('',(6.29,-4.2,-0.1));
#5572=CARTESIAN_POINT('Origin',(6.5,-4.2,1.));
#5573=CARTESIAN_POINT('Origin',(12.,8.,0.));
#5574=CARTESIAN_POINT('',(12.,8.,0.));
#5575=CARTESIAN_POINT('',(-10.,8.,0.));
#5576=CARTESIAN_POINT('',(12.,8.,0.));
#5577=CARTESIAN_POINT('',(-10.,8.,1.));
#5578=CARTESIAN_POINT('',(-10.,8.,0.));
#5579=CARTESIAN_POINT('',(12.,8.,1.));
#5580=CARTESIAN_POINT('',(12.,8.,1.));
#5581=CARTESIAN_POINT('',(12.,8.,0.));
#5582=CARTESIAN_POINT('Origin',(12.,-8.,0.));
#5583=CARTESIAN_POINT('',(12.,-8.,0.));
#5584=CARTESIAN_POINT('',(12.,-8.,0.));
#5585=CARTESIAN_POINT('',(12.,-8.,1.));
#5586=CARTESIAN_POINT('',(12.,-8.,1.));
#5587=CARTESIAN_POINT('',(12.,-8.,0.));
#5588=CARTESIAN_POINT('Origin',(-10.,-8.,0.));
#5589=CARTESIAN_POINT('',(-10.,-8.,0.));
#5590=CARTESIAN_POINT('',(-10.,-8.,0.));
#5591=CARTESIAN_POINT('',(-10.,-8.,1.));
#5592=CARTESIAN_POINT('',(-10.,-8.,1.));
#5593=CARTESIAN_POINT('',(-10.,-8.,0.));
#5594=CARTESIAN_POINT('Origin',(-10.,8.,0.));
#5595=CARTESIAN_POINT('',(-10.,8.,0.));
#5596=CARTESIAN_POINT('',(-10.,8.,1.));
#5597=CARTESIAN_POINT('Origin',(1.,0.,1.));
#5598=CARTESIAN_POINT('Origin',(1.,0.,0.));
#5599=CARTESIAN_POINT('',(0.,0.,0.));
#5600=CARTESIAN_POINT('Origin',(-9.,-7.,-0.5));
#5601=CARTESIAN_POINT('',(-9.8,-7.,0.));
#5602=CARTESIAN_POINT('Origin',(-9.,-7.,0.));
#5603=CARTESIAN_POINT('',(-9.8,-7.,-0.5));
#5604=CARTESIAN_POINT('',(-9.8,-7.,-0.5));
#5605=CARTESIAN_POINT('Origin',(-9.,-7.,-0.5));
#5606=CARTESIAN_POINT('Origin',(-9.,-7.,0.));
#5607=CARTESIAN_POINT('Origin',(-9.,-7.,-0.5));
#5608=CARTESIAN_POINT('',(0.,0.,0.));
#5609=CARTESIAN_POINT('Origin',(-9.,7.,-0.5));
#5610=CARTESIAN_POINT('',(-9.8,7.,0.));
#5611=CARTESIAN_POINT('Origin',(-9.,7.,0.));
#5612=CARTESIAN_POINT('',(-9.8,7.,-0.5));
#5613=CARTESIAN_POINT('',(-9.8,7.,-0.5));
#5614=CARTESIAN_POINT('Origin',(-9.,7.,-0.5));
#5615=CARTESIAN_POINT('Origin',(-9.,7.,0.));
#5616=CARTESIAN_POINT('Origin',(-9.,7.,-0.5));
#5617=CARTESIAN_POINT('',(0.,0.,0.));
#5618=CARTESIAN_POINT('Origin',(11.,-7.,-0.5));
#5619=CARTESIAN_POINT('',(10.2,-7.,0.));
#5620=CARTESIAN_POINT('Origin',(11.,-7.,0.));
#5621=CARTESIAN_POINT('',(10.2,-7.,-0.5));
#5622=CARTESIAN_POINT('',(10.2,-7.,-0.5));
#5623=CARTESIAN_POINT('Origin',(11.,-7.,-0.5));
#5624=CARTESIAN_POINT('Origin',(11.,-7.,0.));
#5625=CARTESIAN_POINT('Origin',(11.,-7.,-0.5));
#5626=CARTESIAN_POINT('',(0.,0.,0.));
#5627=CARTESIAN_POINT('Origin',(11.,7.,-0.5));
#5628=CARTESIAN_POINT('',(10.2,7.,0.));
#5629=CARTESIAN_POINT('Origin',(11.,7.,0.));
#5630=CARTESIAN_POINT('',(10.2,7.,-0.5));
#5631=CARTESIAN_POINT('',(10.2,7.,-0.5));
#5632=CARTESIAN_POINT('Origin',(11.,7.,-0.5));
#5633=CARTESIAN_POINT('Origin',(11.,7.,0.));
#5634=CARTESIAN_POINT('Origin',(11.,7.,-0.5));
#5635=CARTESIAN_POINT('',(0.,0.,0.));
#5636=CARTESIAN_POINT('Origin',(3.5,-1.8,1.8));
#5637=CARTESIAN_POINT('',(3.05,-1.8,1.8));
#5638=CARTESIAN_POINT('Origin',(3.5,-1.8,1.8));
#5639=CARTESIAN_POINT('',(3.05,-1.8,2.5));
#5640=CARTESIAN_POINT('',(3.05,-1.8,1.8));
#5641=CARTESIAN_POINT('Origin',(3.5,-1.8,2.5));
#5642=CARTESIAN_POINT('Origin',(3.5,-1.8,1.8));
#5643=CARTESIAN_POINT('',(3.225,-1.8,1.8));
#5644=CARTESIAN_POINT('Origin',(3.5,-1.8,1.8));
#5645=CARTESIAN_POINT('Origin',(-3.5,1.8,1.8));
#5646=CARTESIAN_POINT('',(-3.95,1.8,1.8));
#5647=CARTESIAN_POINT('Origin',(-3.5,1.8,1.8));
#5648=CARTESIAN_POINT('',(-3.95,1.8,2.5));
#5649=CARTESIAN_POINT('',(-3.95,1.8,1.8));
#5650=CARTESIAN_POINT('Origin',(-3.5,1.8,2.5));
#5651=CARTESIAN_POINT('Origin',(-3.5,1.8,1.8));
#5652=CARTESIAN_POINT('',(-3.775,1.8,1.8));
#5653=CARTESIAN_POINT('Origin',(-3.5,1.8,1.8));
#5654=CARTESIAN_POINT('Origin',(-3.5,-1.8,1.8));
#5655=CARTESIAN_POINT('',(-3.95,-1.8,1.8));
#5656=CARTESIAN_POINT('Origin',(-3.5,-1.8,1.8));
#5657=CARTESIAN_POINT('',(-3.95,-1.8,2.5));
#5658=CARTESIAN_POINT('',(-3.95,-1.8,1.8));
#5659=CARTESIAN_POINT('Origin',(-3.5,-1.8,2.5));
#5660=CARTESIAN_POINT('Origin',(-3.5,-1.8,1.8));
#5661=CARTESIAN_POINT('',(-3.775,-1.8,1.8));
#5662=CARTESIAN_POINT('Origin',(-3.5,-1.8,1.8));
#5663=CARTESIAN_POINT('Origin',(3.5,1.8,1.8));
#5664=CARTESIAN_POINT('',(3.05,1.8,1.8));
#5665=CARTESIAN_POINT('Origin',(3.5,1.8,1.8));
#5666=CARTESIAN_POINT('',(3.05,1.8,2.5));
#5667=CARTESIAN_POINT('',(3.05,1.8,1.8));
#5668=CARTESIAN_POINT('Origin',(3.5,1.8,2.5));
#5669=CARTESIAN_POINT('Origin',(3.5,1.8,1.8));
#5670=CARTESIAN_POINT('',(3.225,1.8,1.8));
#5671=CARTESIAN_POINT('Origin',(3.5,1.8,1.8));
#5672=CARTESIAN_POINT('Origin',(3.5,-1.8,0.9));
#5673=CARTESIAN_POINT('',(3.225,-1.8,1.));
#5674=CARTESIAN_POINT('Origin',(3.5,-1.8,1.));
#5675=CARTESIAN_POINT('',(3.225,-1.8,0.9));
#5676=CARTESIAN_POINT('Origin',(-3.5,1.8,0.9));
#5677=CARTESIAN_POINT('',(-3.775,1.8,1.));
#5678=CARTESIAN_POINT('Origin',(-3.5,1.8,1.));
#5679=CARTESIAN_POINT('',(-3.775,1.8,0.9));
#5680=CARTESIAN_POINT('Origin',(-3.5,-1.8,0.9));
#5681=CARTESIAN_POINT('',(-3.775,-1.8,1.));
#5682=CARTESIAN_POINT('Origin',(-3.5,-1.8,1.));
#5683=CARTESIAN_POINT('',(-3.775,-1.8,0.9));
#5684=CARTESIAN_POINT('Origin',(3.5,1.8,0.9));
#5685=CARTESIAN_POINT('',(3.225,1.8,1.));
#5686=CARTESIAN_POINT('Origin',(3.5,1.8,1.));
#5687=CARTESIAN_POINT('',(3.225,1.8,0.9));
#5688=CARTESIAN_POINT('Origin',(-3.,-1.5,1.5));
#5689=CARTESIAN_POINT('',(3.,-1.5,2.5));
#5690=CARTESIAN_POINT('',(-3.,-1.5,2.5));
#5691=CARTESIAN_POINT('',(-1.5,-1.5,2.5));
#5692=CARTESIAN_POINT('',(3.,-1.5,1.5));
#5693=CARTESIAN_POINT('',(3.,-1.5,1.5));
#5694=CARTESIAN_POINT('',(-3.,-1.5,1.5));
#5695=CARTESIAN_POINT('',(-3.,-1.5,1.5));
#5696=CARTESIAN_POINT('',(-3.,-1.5,1.5));
#5697=CARTESIAN_POINT('Origin',(-3.,1.5,1.5));
#5698=CARTESIAN_POINT('',(-3.,1.5,2.5));
#5699=CARTESIAN_POINT('',(-3.,0.75,2.5));
#5700=CARTESIAN_POINT('',(-3.,1.5,1.5));
#5701=CARTESIAN_POINT('',(-3.,1.5,1.5));
#5702=CARTESIAN_POINT('',(-3.,1.5,1.5));
#5703=CARTESIAN_POINT('Origin',(3.,1.5,1.5));
#5704=CARTESIAN_POINT('',(3.,1.5,2.5));
#5705=CARTESIAN_POINT('',(1.5,1.5,2.5));
#5706=CARTESIAN_POINT('',(3.,1.5,1.5));
#5707=CARTESIAN_POINT('',(3.,1.5,1.5));
#5708=CARTESIAN_POINT('',(3.,1.5,1.5));
#5709=CARTESIAN_POINT('Origin',(3.,-1.5,1.5));
#5710=CARTESIAN_POINT('',(3.,-0.75,2.5));
#5711=CARTESIAN_POINT('',(3.,-1.5,1.5));
#5712=CARTESIAN_POINT('Origin',(0.,0.,1.5));
#5713=CARTESIAN_POINT('Origin',(4.,2.5,1.));
#5714=CARTESIAN_POINT('',(4.,2.5,1.));
#5715=CARTESIAN_POINT('',(-4.,2.5,1.));
#5716=CARTESIAN_POINT('',(4.,2.5,1.));
#5717=CARTESIAN_POINT('',(-4.,2.5,2.5));
#5718=CARTESIAN_POINT('',(-4.,2.5,1.));
#5719=CARTESIAN_POINT('',(4.,2.5,2.5));
#5720=CARTESIAN_POINT('',(4.,2.5,2.5));
#5721=CARTESIAN_POINT('',(4.,2.5,1.));
#5722=CARTESIAN_POINT('Origin',(4.,-2.5,1.));
#5723=CARTESIAN_POINT('',(4.,-2.5,1.));
#5724=CARTESIAN_POINT('',(4.,-2.5,1.));
#5725=CARTESIAN_POINT('',(4.,-2.5,2.5));
#5726=CARTESIAN_POINT('',(4.,-2.5,2.5));
#5727=CARTESIAN_POINT('',(4.,-2.5,1.));
#5728=CARTESIAN_POINT('Origin',(-4.,-2.5,1.));
#5729=CARTESIAN_POINT('',(-4.,-2.5,1.));
#5730=CARTESIAN_POINT('',(-4.,-2.5,1.));
#5731=CARTESIAN_POINT('',(-4.,-2.5,2.5));
#5732=CARTESIAN_POINT('',(-4.,-2.5,2.5));
#5733=CARTESIAN_POINT('',(-4.,-2.5,1.));
#5734=CARTESIAN_POINT('Origin',(-4.,2.5,1.));
#5735=CARTESIAN_POINT('',(-4.,2.5,1.));
#5736=CARTESIAN_POINT('',(-4.,2.5,2.5));
#5737=CARTESIAN_POINT('Origin',(0.,0.,2.5));
#5738=CARTESIAN_POINT('Origin',(0.,0.,1.));
#5739=CARTESIAN_POINT('',(0.,0.,0.));
#5740=CARTESIAN_POINT('Origin',(3.,1.5,1.5));
#5741=CARTESIAN_POINT('',(3.,1.5,1.5));
#5742=CARTESIAN_POINT('',(-3.,1.5,1.5));
#5743=CARTESIAN_POINT('',(3.,1.5,1.5));
#5744=CARTESIAN_POINT('',(-3.,1.5,2.5));
#5745=CARTESIAN_POINT('',(-3.,1.5,1.5));
#5746=CARTESIAN_POINT('',(3.,1.5,2.5));
#5747=CARTESIAN_POINT('',(3.,1.5,2.5));
#5748=CARTESIAN_POINT('',(3.,1.5,1.5));
#5749=CARTESIAN_POINT('Origin',(3.,-1.5,1.5));
#5750=CARTESIAN_POINT('',(3.,-1.5,1.5));
#5751=CARTESIAN_POINT('',(3.,-1.5,1.5));
#5752=CARTESIAN_POINT('',(3.,-1.5,2.5));
#5753=CARTESIAN_POINT('',(3.,-1.5,2.5));
#5754=CARTESIAN_POINT('',(3.,-1.5,1.5));
#5755=CARTESIAN_POINT('Origin',(-3.,-1.5,1.5));
#5756=CARTESIAN_POINT('',(-3.,-1.5,1.5));
#5757=CARTESIAN_POINT('',(-3.,-1.5,1.5));
#5758=CARTESIAN_POINT('',(-3.,-1.5,2.5));
#5759=CARTESIAN_POINT('',(-3.,-1.5,2.5));
#5760=CARTESIAN_POINT('',(-3.,-1.5,1.5));
#5761=CARTESIAN_POINT('Origin',(-3.,1.5,1.5));
#5762=CARTESIAN_POINT('',(-3.,1.5,1.5));
#5763=CARTESIAN_POINT('',(-3.,1.5,2.5));
#5764=CARTESIAN_POINT('Origin',(0.,0.,2.5));
#5765=CARTESIAN_POINT('Origin',(0.,0.,1.5));
#5766=CARTESIAN_POINT('',(0.,0.,0.));
#5767=CARTESIAN_POINT('Origin',(-6.5,-6.5,1.8));
#5768=CARTESIAN_POINT('',(-6.975,-6.5,1.8));
#5769=CARTESIAN_POINT('Origin',(-6.5,-6.5,1.8));
#5770=CARTESIAN_POINT('',(-6.975,-6.5,4.5));
#5771=CARTESIAN_POINT('',(-6.975,-6.5,1.8));
#5772=CARTESIAN_POINT('Origin',(-6.5,-6.5,4.5));
#5773=CARTESIAN_POINT('',(-6.9654030511288,-6.405,3.5));
#5774=CARTESIAN_POINT('Ctrl Pts',(-6.9654030511288,-6.405,3.5));
#5775=CARTESIAN_POINT('Ctrl Pts',(-6.9654030511288,-6.405,3.44082671433706));
#5776=CARTESIAN_POINT('Ctrl Pts',(-6.96319194510978,-6.391162819218,3.3786038562345));
#5777=CARTESIAN_POINT('Ctrl Pts',(-6.9474004570938,-6.33805779261652,3.26878119899199));
#5778=CARTESIAN_POINT('Ctrl Pts',(-6.93296763252909,-6.29875591394082,3.22132213181236));
#5779=CARTESIAN_POINT('Ctrl Pts',(-6.89697744222372,-6.23823300006139,3.17155768103299));
#5780=CARTESIAN_POINT('Ctrl Pts',(-6.88237408148839,-6.2169021926909,3.15715697182391));
#5781=CARTESIAN_POINT('Ctrl Pts',(-6.84782319019902,-6.17538739566531,3.13417605500228));
#5782=CARTESIAN_POINT('Ctrl Pts',(-6.8278469830262,-6.1552757719279,3.12550838237099));
#5783=CARTESIAN_POINT('Ctrl Pts',(-6.76795622589237,-6.10432382827604,3.1070097286502));
#5784=CARTESIAN_POINT('Ctrl Pts',(-6.71846870594364,-6.07437258197005,3.10138466314703));
#5785=CARTESIAN_POINT('Ctrl Pts',(-6.61134072173687,-6.03471454832095,3.09599463066268));
#5786=CARTESIAN_POINT('Ctrl Pts',(-6.55372663006585,-6.025,3.09577234137185));
#5787=CARTESIAN_POINT('Ctrl Pts',(-6.44627336993415,-6.025,3.09577234137185));
#5788=CARTESIAN_POINT('Ctrl Pts',(-6.38865927826313,-6.03471454832095,3.09599463066268));
#5789=CARTESIAN_POINT('Ctrl Pts',(-6.28153129405636,-6.07437258197005,3.10138466314702));
#5790=CARTESIAN_POINT('Ctrl Pts',(-6.23204377410763,-6.10432382827604,3.1070097286502));
#5791=CARTESIAN_POINT('Ctrl Pts',(-6.1721530169738,-6.1552757719279,3.12550838237099));
#5792=CARTESIAN_POINT('Ctrl Pts',(-6.15217680980098,-6.17538739566531,3.13417605500228));
#5793=CARTESIAN_POINT('Ctrl Pts',(-6.11762591851161,-6.2169021926909,3.15715697182391));
#5794=CARTESIAN_POINT('Ctrl Pts',(-6.10302255777628,-6.23823300006139,3.17155768103299));
#5795=CARTESIAN_POINT('Ctrl Pts',(-6.06703236747091,-6.29875591394082,3.22132213181236));
#5796=CARTESIAN_POINT('Ctrl Pts',(-6.0525995429062,-6.33805779261652,3.26878119899199));
#5797=CARTESIAN_POINT('Ctrl Pts',(-6.03680805489022,-6.391162819218,3.3786038562345));
#5798=CARTESIAN_POINT('Ctrl Pts',(-6.0345969488712,-6.405,3.44082671433706));
#5799=CARTESIAN_POINT('Ctrl Pts',(-6.0345969488712,-6.405,3.55917328566294));
#5800=CARTESIAN_POINT('Ctrl Pts',(-6.03680805489022,-6.391162819218,3.6213961437655));
#5801=CARTESIAN_POINT('Ctrl Pts',(-6.0525995429062,-6.33805779261652,3.73121880100801));
#5802=CARTESIAN_POINT('Ctrl Pts',(-6.06703236747091,-6.29875591394082,3.77867786818764));
#5803=CARTESIAN_POINT('Ctrl Pts',(-6.10302255777628,-6.23823300006139,3.82844231896701));
#5804=CARTESIAN_POINT('Ctrl Pts',(-6.1176259185116,-6.2169021926909,3.84284302817609));
#5805=CARTESIAN_POINT('Ctrl Pts',(-6.15217680980098,-6.17538739566531,3.86582394499772));
#5806=CARTESIAN_POINT('Ctrl Pts',(-6.1721530169738,-6.1552757719279,3.87449161762901));
#5807=CARTESIAN_POINT('Ctrl Pts',(-6.23204377410763,-6.10432382827604,3.8929902713498));
#5808=CARTESIAN_POINT('Ctrl Pts',(-6.28153129405636,-6.07437258197005,3.89861533685297));
#5809=CARTESIAN_POINT('Ctrl Pts',(-6.38865927826313,-6.03471454832095,3.90400536933732));
#5810=CARTESIAN_POINT('Ctrl Pts',(-6.44627336993415,-6.025,3.90422765862815));
#5811=CARTESIAN_POINT('Ctrl Pts',(-6.55372663006585,-6.025,3.90422765862815));
#5812=CARTESIAN_POINT('Ctrl Pts',(-6.61134072173687,-6.03471454832095,3.90400536933732));
#5813=CARTESIAN_POINT('Ctrl Pts',(-6.71846870594364,-6.07437258197005,3.89861533685297));
#5814=CARTESIAN_POINT('Ctrl Pts',(-6.76795622589237,-6.10432382827604,3.8929902713498));
#5815=CARTESIAN_POINT('Ctrl Pts',(-6.8278469830262,-6.1552757719279,3.87449161762901));
#5816=CARTESIAN_POINT('Ctrl Pts',(-6.84782319019902,-6.17538739566531,3.86582394499772));
#5817=CARTESIAN_POINT('Ctrl Pts',(-6.8823740814884,-6.21690219269089,3.84284302817609));
#5818=CARTESIAN_POINT('Ctrl Pts',(-6.89697744222372,-6.23823300006139,3.82844231896701));
#5819=CARTESIAN_POINT('Ctrl Pts',(-6.93296763252909,-6.29875591394082,3.77867786818764));
#5820=CARTESIAN_POINT('Ctrl Pts',(-6.9474004570938,-6.33805779261652,3.73121880100801));
#5821=CARTESIAN_POINT('Ctrl Pts',(-6.96319194510978,-6.391162819218,3.6213961437655));
#5822=CARTESIAN_POINT('Ctrl Pts',(-6.9654030511288,-6.405,3.55917328566294));
#5823=CARTESIAN_POINT('Ctrl Pts',(-6.9654030511288,-6.405,3.5));
#5824=CARTESIAN_POINT('Origin',(-6.5,-6.5,1.8));
#5825=CARTESIAN_POINT('',(-6.775,-6.5,1.8));
#5826=CARTESIAN_POINT('Origin',(-6.5,-6.5,1.8));
#5827=CARTESIAN_POINT('Origin',(-6.5,-6.5,0.9));
#5828=CARTESIAN_POINT('',(-6.775,-6.5,1.));
#5829=CARTESIAN_POINT('Origin',(-6.5,-6.5,1.));
#5830=CARTESIAN_POINT('',(-6.775,-6.5,0.9));
#5831=CARTESIAN_POINT('Origin',(-6.5,-4.2,0.9));
#5832=CARTESIAN_POINT('',(-6.775,-4.2,1.));
#5833=CARTESIAN_POINT('Origin',(-6.5,-4.2,1.));
#5834=CARTESIAN_POINT('',(-6.775,-4.2,1.8));
#5835=CARTESIAN_POINT('',(-6.775,-4.2,0.9));
#5836=CARTESIAN_POINT('Origin',(-6.5,-4.2,1.8));
#5837=CARTESIAN_POINT('Origin',(-7.1,-6.,3.5));
#5838=CARTESIAN_POINT('',(-7.,-6.,3.905));
#5839=CARTESIAN_POINT('Origin',(-7.,-6.,3.5));
#5840=CARTESIAN_POINT('',(-6.,-6.,3.905));
#5841=CARTESIAN_POINT('',(-7.1,-6.,3.905));
#5842=CARTESIAN_POINT('Origin',(-6.,-6.,3.5));
#5843=CARTESIAN_POINT('Origin',(-7.,-5.,4.5));
#5844=CARTESIAN_POINT('',(-7.,-5.,4.5));
#5845=CARTESIAN_POINT('',(-7.,-7.,4.5));
#5846=CARTESIAN_POINT('',(-7.,-5.,4.5));
#5847=CARTESIAN_POINT('',(-6.,-7.,4.5));
#5848=CARTESIAN_POINT('',(-7.,-7.,4.5));
#5849=CARTESIAN_POINT('',(-6.,-5.,4.5));
#5850=CARTESIAN_POINT('',(-6.,-5.,4.5));
#5851=CARTESIAN_POINT('',(-7.,-5.,4.5));
#5852=CARTESIAN_POINT('Origin',(-7.,-5.,1.8));
#5853=CARTESIAN_POINT('',(-7.,-5.,1.8));
#5854=CARTESIAN_POINT('',(-7.,-5.,1.8));
#5855=CARTESIAN_POINT('',(-6.,-5.,1.8));
#5856=CARTESIAN_POINT('',(-6.,-5.,1.8));
#5857=CARTESIAN_POINT('',(-7.,-5.,1.8));
#5858=CARTESIAN_POINT('Origin',(-7.,-3.5,1.8));
#5859=CARTESIAN_POINT('',(-7.,-3.5,1.8));
#5860=CARTESIAN_POINT('',(-7.,-3.5,1.8));
#5861=CARTESIAN_POINT('',(-6.,-3.5,1.8));
#5862=CARTESIAN_POINT('',(-6.,-3.5,1.8));
#5863=CARTESIAN_POINT('',(-7.,-3.5,1.8));
#5864=CARTESIAN_POINT('Origin',(-7.,-3.5,1.));
#5865=CARTESIAN_POINT('',(-7.,-3.5,1.));
#5866=CARTESIAN_POINT('',(-7.,-3.5,1.));
#5867=CARTESIAN_POINT('',(-6.,-3.5,1.));
#5868=CARTESIAN_POINT('',(-6.,-3.5,1.));
#5869=CARTESIAN_POINT('',(-7.,-3.5,1.));
#5870=CARTESIAN_POINT('Origin',(-7.,-7.,1.));
#5871=CARTESIAN_POINT('',(-7.,-7.,1.));
#5872=CARTESIAN_POINT('',(-7.,-7.,1.));
#5873=CARTESIAN_POINT('',(-6.,-7.,1.));
#5874=CARTESIAN_POINT('',(-6.,-7.,1.));
#5875=CARTESIAN_POINT('',(-7.,-7.,1.));
#5876=CARTESIAN_POINT('Origin',(-7.,-7.,4.5));
#5877=CARTESIAN_POINT('',(-7.,-7.,4.5));
#5878=CARTESIAN_POINT('',(-6.,-7.,4.5));
#5879=CARTESIAN_POINT('Origin',(-6.,-5.25,2.75));
#5880=CARTESIAN_POINT('Origin',(-7.,-5.25,2.75));
#5881=CARTESIAN_POINT('',(0.,0.,0.));
#5882=CARTESIAN_POINT('Origin',(6.5,-6.5,1.8));
#5883=CARTESIAN_POINT('',(6.025,-6.5,1.8));
#5884=CARTESIAN_POINT('Origin',(6.5,-6.5,1.8));
#5885=CARTESIAN_POINT('',(6.025,-6.5,4.5));
#5886=CARTESIAN_POINT('',(6.025,-6.5,1.8));
#5887=CARTESIAN_POINT('Origin',(6.5,-6.5,4.5));
#5888=CARTESIAN_POINT('',(6.0345969488712,-6.405,3.5));
#5889=CARTESIAN_POINT('Ctrl Pts',(6.0345969488712,-6.405,3.5));
#5890=CARTESIAN_POINT('Ctrl Pts',(6.0345969488712,-6.405,3.44082671433706));
#5891=CARTESIAN_POINT('Ctrl Pts',(6.03680805489022,-6.391162819218,3.3786038562345));
#5892=CARTESIAN_POINT('Ctrl Pts',(6.0525995429062,-6.33805779261652,3.26878119899199));
#5893=CARTESIAN_POINT('Ctrl Pts',(6.06703236747091,-6.29875591394082,3.22132213181236));
#5894=CARTESIAN_POINT('Ctrl Pts',(6.10302255777628,-6.23823300006139,3.17155768103299));
#5895=CARTESIAN_POINT('Ctrl Pts',(6.11762591851161,-6.2169021926909,3.15715697182391));
#5896=CARTESIAN_POINT('Ctrl Pts',(6.15217680980098,-6.17538739566531,3.13417605500228));
#5897=CARTESIAN_POINT('Ctrl Pts',(6.1721530169738,-6.1552757719279,3.12550838237099));
#5898=CARTESIAN_POINT('Ctrl Pts',(6.23204377410763,-6.10432382827604,3.1070097286502));
#5899=CARTESIAN_POINT('Ctrl Pts',(6.28153129405636,-6.07437258197005,3.10138466314703));
#5900=CARTESIAN_POINT('Ctrl Pts',(6.38865927826313,-6.03471454832095,3.09599463066268));
#5901=CARTESIAN_POINT('Ctrl Pts',(6.44627336993415,-6.025,3.09577234137185));
#5902=CARTESIAN_POINT('Ctrl Pts',(6.55372663006585,-6.025,3.09577234137185));
#5903=CARTESIAN_POINT('Ctrl Pts',(6.61134072173687,-6.03471454832095,3.09599463066268));
#5904=CARTESIAN_POINT('Ctrl Pts',(6.71846870594365,-6.07437258197005,3.10138466314703));
#5905=CARTESIAN_POINT('Ctrl Pts',(6.76795622589237,-6.10432382827604,3.1070097286502));
#5906=CARTESIAN_POINT('Ctrl Pts',(6.8278469830262,-6.1552757719279,3.12550838237099));
#5907=CARTESIAN_POINT('Ctrl Pts',(6.84782319019902,-6.17538739566531,3.13417605500228));
#5908=CARTESIAN_POINT('Ctrl Pts',(6.88237408148839,-6.2169021926909,3.15715697182391));
#5909=CARTESIAN_POINT('Ctrl Pts',(6.89697744222372,-6.23823300006139,3.17155768103299));
#5910=CARTESIAN_POINT('Ctrl Pts',(6.93296763252909,-6.29875591394082,3.22132213181236));
#5911=CARTESIAN_POINT('Ctrl Pts',(6.9474004570938,-6.33805779261652,3.26878119899199));
#5912=CARTESIAN_POINT('Ctrl Pts',(6.96319194510978,-6.391162819218,3.3786038562345));
#5913=CARTESIAN_POINT('Ctrl Pts',(6.9654030511288,-6.405,3.44082671433706));
#5914=CARTESIAN_POINT('Ctrl Pts',(6.9654030511288,-6.405,3.55917328566294));
#5915=CARTESIAN_POINT('Ctrl Pts',(6.96319194510978,-6.391162819218,3.6213961437655));
#5916=CARTESIAN_POINT('Ctrl Pts',(6.9474004570938,-6.33805779261652,3.73121880100801));
#5917=CARTESIAN_POINT('Ctrl Pts',(6.93296763252909,-6.29875591394082,3.77867786818764));
#5918=CARTESIAN_POINT('Ctrl Pts',(6.89697744222372,-6.23823300006139,3.82844231896701));
#5919=CARTESIAN_POINT('Ctrl Pts',(6.8823740814884,-6.2169021926909,3.84284302817609));
#5920=CARTESIAN_POINT('Ctrl Pts',(6.84782319019902,-6.17538739566531,3.86582394499772));
#5921=CARTESIAN_POINT('Ctrl Pts',(6.8278469830262,-6.1552757719279,3.87449161762901));
#5922=CARTESIAN_POINT('Ctrl Pts',(6.76795622589237,-6.10432382827604,3.8929902713498));
#5923=CARTESIAN_POINT('Ctrl Pts',(6.71846870594364,-6.07437258197005,3.89861533685297));
#5924=CARTESIAN_POINT('Ctrl Pts',(6.61134072173687,-6.03471454832095,3.90400536933732));
#5925=CARTESIAN_POINT('Ctrl Pts',(6.55372663006585,-6.025,3.90422765862815));
#5926=CARTESIAN_POINT('Ctrl Pts',(6.44627336993415,-6.025,3.90422765862815));
#5927=CARTESIAN_POINT('Ctrl Pts',(6.38865927826313,-6.03471454832095,3.90400536933732));
#5928=CARTESIAN_POINT('Ctrl Pts',(6.28153129405636,-6.07437258197005,3.89861533685297));
#5929=CARTESIAN_POINT('Ctrl Pts',(6.23204377410763,-6.10432382827604,3.8929902713498));
#5930=CARTESIAN_POINT('Ctrl Pts',(6.1721530169738,-6.1552757719279,3.87449161762901));
#5931=CARTESIAN_POINT('Ctrl Pts',(6.15217680980098,-6.17538739566531,3.86582394499772));
#5932=CARTESIAN_POINT('Ctrl Pts',(6.1176259185116,-6.2169021926909,3.84284302817609));
#5933=CARTESIAN_POINT('Ctrl Pts',(6.10302255777628,-6.23823300006139,3.82844231896701));
#5934=CARTESIAN_POINT('Ctrl Pts',(6.06703236747091,-6.29875591394082,3.77867786818764));
#5935=CARTESIAN_POINT('Ctrl Pts',(6.0525995429062,-6.33805779261652,3.73121880100801));
#5936=CARTESIAN_POINT('Ctrl Pts',(6.03680805489022,-6.391162819218,3.6213961437655));
#5937=CARTESIAN_POINT('Ctrl Pts',(6.0345969488712,-6.405,3.55917328566294));
#5938=CARTESIAN_POINT('Ctrl Pts',(6.0345969488712,-6.405,3.5));
#5939=CARTESIAN_POINT('Origin',(6.5,-6.5,1.8));
#5940=CARTESIAN_POINT('',(6.225,-6.5,1.8));
#5941=CARTESIAN_POINT('Origin',(6.5,-6.5,1.8));
#5942=CARTESIAN_POINT('Origin',(6.5,-6.5,0.9));
#5943=CARTESIAN_POINT('',(6.225,-6.5,1.));
#5944=CARTESIAN_POINT('Origin',(6.5,-6.5,1.));
#5945=CARTESIAN_POINT('',(6.225,-6.5,0.9));
#5946=CARTESIAN_POINT('Origin',(6.5,-4.2,0.9));
#5947=CARTESIAN_POINT('',(6.225,-4.2,1.));
#5948=CARTESIAN_POINT('Origin',(6.5,-4.2,1.));
#5949=CARTESIAN_POINT('',(6.225,-4.2,1.8));
#5950=CARTESIAN_POINT('',(6.225,-4.2,0.9));
#5951=CARTESIAN_POINT('Origin',(6.5,-4.2,1.8));
#5952=CARTESIAN_POINT('Origin',(5.9,-6.,3.5));
#5953=CARTESIAN_POINT('',(6.,-6.,3.905));
#5954=CARTESIAN_POINT('Origin',(6.,-6.,3.5));
#5955=CARTESIAN_POINT('',(7.,-6.,3.905));
#5956=CARTESIAN_POINT('',(5.9,-6.,3.905));
#5957=CARTESIAN_POINT('Origin',(7.,-6.,3.5));
#5958=CARTESIAN_POINT('Origin',(6.,-5.,4.5));
#5959=CARTESIAN_POINT('',(6.,-5.,4.5));
#5960=CARTESIAN_POINT('',(6.,-7.,4.5));
#5961=CARTESIAN_POINT('',(6.,-5.,4.5));
#5962=CARTESIAN_POINT('',(7.,-7.,4.5));
#5963=CARTESIAN_POINT('',(6.,-7.,4.5));
#5964=CARTESIAN_POINT('',(7.,-5.,4.5));
#5965=CARTESIAN_POINT('',(7.,-5.,4.5));
#5966=CARTESIAN_POINT('',(6.,-5.,4.5));
#5967=CARTESIAN_POINT('Origin',(6.,-5.,1.8));
#5968=CARTESIAN_POINT('',(6.,-5.,1.8));
#5969=CARTESIAN_POINT('',(6.,-5.,1.8));
#5970=CARTESIAN_POINT('',(7.,-5.,1.8));
#5971=CARTESIAN_POINT('',(7.,-5.,1.8));
#5972=CARTESIAN_POINT('',(6.,-5.,1.8));
#5973=CARTESIAN_POINT('Origin',(6.,-3.5,1.8));
#5974=CARTESIAN_POINT('',(6.,-3.5,1.8));
#5975=CARTESIAN_POINT('',(6.,-3.5,1.8));
#5976=CARTESIAN_POINT('',(7.,-3.5,1.8));
#5977=CARTESIAN_POINT('',(7.,-3.5,1.8));
#5978=CARTESIAN_POINT('',(6.,-3.5,1.8));
#5979=CARTESIAN_POINT('Origin',(6.,-3.5,1.));
#5980=CARTESIAN_POINT('',(6.,-3.5,1.));
#5981=CARTESIAN_POINT('',(6.,-3.5,1.));
#5982=CARTESIAN_POINT('',(7.,-3.5,1.));
#5983=CARTESIAN_POINT('',(7.,-3.5,1.));
#5984=CARTESIAN_POINT('',(6.,-3.5,1.));
#5985=CARTESIAN_POINT('Origin',(6.,-7.,1.));
#5986=CARTESIAN_POINT('',(6.,-7.,1.));
#5987=CARTESIAN_POINT('',(6.,-7.,1.));
#5988=CARTESIAN_POINT('',(7.,-7.,1.));
#5989=CARTESIAN_POINT('',(7.,-7.,1.));
#5990=CARTESIAN_POINT('',(6.,-7.,1.));
#5991=CARTESIAN_POINT('Origin',(6.,-7.,4.5));
#5992=CARTESIAN_POINT('',(6.,-7.,4.5));
#5993=CARTESIAN_POINT('',(7.,-7.,4.5));
#5994=CARTESIAN_POINT('Origin',(7.,-5.25,2.75));
#5995=CARTESIAN_POINT('Origin',(6.,-5.25,2.75));
#5996=CARTESIAN_POINT('',(0.,0.,0.));
#5997=CARTESIAN_POINT('Origin',(6.,-6.,3.5));
#5998=CARTESIAN_POINT('',(6.,-6.,3.665));
#5999=CARTESIAN_POINT('Origin',(6.,-6.,3.5));
#6000=CARTESIAN_POINT('',(7.6,-6.,3.665));
#6001=CARTESIAN_POINT('',(6.,-6.,3.665));
#6002=CARTESIAN_POINT('Origin',(7.6,-6.,3.5));
#6003=CARTESIAN_POINT('Origin',(6.,-6.,3.5));
#6004=CARTESIAN_POINT('Origin',(-7.7,-6.,3.5));
#6005=CARTESIAN_POINT('',(-7.6,-6.,3.665));
#6006=CARTESIAN_POINT('Origin',(-7.6,-6.,3.5));
#6007=CARTESIAN_POINT('',(-6.,-6.,3.665));
#6008=CARTESIAN_POINT('',(-7.7,-6.,3.665));
#6009=CARTESIAN_POINT('Origin',(-6.,-6.,3.5));
#6010=CARTESIAN_POINT('Origin',(-6.,-6.,3.5));
#6011=CARTESIAN_POINT('Origin',(-7.6,-6.,3.5));
#6012=CARTESIAN_POINT('',(7.6,-6.,3.9));
#6013=CARTESIAN_POINT('Origin',(7.6,-6.,3.5));
#6014=CARTESIAN_POINT('',(-7.6,-6.,3.9));
#6015=CARTESIAN_POINT('',(-7.6,-6.,3.9));
#6016=CARTESIAN_POINT('Origin',(-7.6,-6.,3.5));
#6017=CARTESIAN_POINT('Origin',(7.6,-6.,3.5));
#6018=CARTESIAN_POINT('Origin',(-7.6,-6.,3.5));
#6019=CARTESIAN_POINT('',(0.,0.,0.));
#6020=CARTESIAN_POINT('Origin',(-7.8,-6.,3.5));
#6021=CARTESIAN_POINT('',(-7.6,-6.,3.725));
#6022=CARTESIAN_POINT('Origin',(-7.6,-6.,3.5));
#6023=CARTESIAN_POINT('',(-7.8,-6.,3.725));
#6024=CARTESIAN_POINT('',(-7.8,-6.,3.725));
#6025=CARTESIAN_POINT('Origin',(-7.8,-6.,3.5));
#6026=CARTESIAN_POINT('Origin',(-7.8,-6.,3.5));
#6027=CARTESIAN_POINT('',(-7.6,-6.,4.3));
#6028=CARTESIAN_POINT('Origin',(-7.6,-6.,3.5));
#6029=CARTESIAN_POINT('',(-7.8,-6.,4.3));
#6030=CARTESIAN_POINT('',(-7.8,-6.,4.3));
#6031=CARTESIAN_POINT('Origin',(-7.8,-6.,3.5));
#6032=CARTESIAN_POINT('Origin',(-7.6,-6.,3.5));
#6033=CARTESIAN_POINT('Origin',(-7.8,-6.,3.5));
#6034=CARTESIAN_POINT('',(0.,0.,0.));
#6035=CARTESIAN_POINT('Origin',(7.6,-6.,3.5));
#6036=CARTESIAN_POINT('',(7.8,-6.,3.725));
#6037=CARTESIAN_POINT('Origin',(7.8,-6.,3.5));
#6038=CARTESIAN_POINT('',(7.6,-6.,3.725));
#6039=CARTESIAN_POINT('',(7.6,-6.,3.725));
#6040=CARTESIAN_POINT('Origin',(7.6,-6.,3.5));
#6041=CARTESIAN_POINT('Origin',(7.6,-6.,3.5));
#6042=CARTESIAN_POINT('',(7.8,-6.,4.3));
#6043=CARTESIAN_POINT('Origin',(7.8,-6.,3.5));
#6044=CARTESIAN_POINT('',(7.6,-6.,4.3));
#6045=CARTESIAN_POINT('',(7.6,-6.,4.3));
#6046=CARTESIAN_POINT('Origin',(7.6,-6.,3.5));
#6047=CARTESIAN_POINT('Origin',(7.8,-6.,3.5));
#6048=CARTESIAN_POINT('Origin',(7.6,-6.,3.5));
#6049=CARTESIAN_POINT('',(0.,0.,0.));
#6050=CARTESIAN_POINT('Origin',(9.2,3.5,3.9));
#6051=CARTESIAN_POINT('',(9.035,3.5,3.9));
#6052=CARTESIAN_POINT('Origin',(9.2,3.5,3.9));
#6053=CARTESIAN_POINT('',(9.035,3.5,5.));
#6054=CARTESIAN_POINT('',(9.035,3.5,3.9));
#6055=CARTESIAN_POINT('Origin',(9.2,3.5,5.));
#6056=CARTESIAN_POINT('Origin',(9.2,3.5,3.9));
#6057=CARTESIAN_POINT('Origin',(9.2,2.7,1.6));
#6058=CARTESIAN_POINT('',(9.11097948495089,2.906640625,1.6));
#6059=CARTESIAN_POINT('',(9.28902051504911,2.906640625,1.6));
#6060=CARTESIAN_POINT('Origin',(9.2,3.5,1.6));
#6061=CARTESIAN_POINT('Origin',(9.2,2.7,1.6));
#6062=CARTESIAN_POINT('Origin',(9.2,2.7,0.9));
#6063=CARTESIAN_POINT('',(8.975,2.7,1.));
#6064=CARTESIAN_POINT('Origin',(9.2,2.7,1.));
#6065=CARTESIAN_POINT('',(8.975,2.7,1.5));
#6066=CARTESIAN_POINT('',(8.975,2.7,0.9));
#6067=CARTESIAN_POINT('',(9.28902051504911,2.906640625,1.5));
#6068=CARTESIAN_POINT('Origin',(9.2,2.7,1.5));
#6069=CARTESIAN_POINT('',(9.28902051504911,2.906640625,0.9));
#6070=CARTESIAN_POINT('',(9.11097948495089,2.906640625,1.5));
#6071=CARTESIAN_POINT('',(9.11097948495089,2.906640625,0.9));
#6072=CARTESIAN_POINT('Origin',(9.2,2.7,1.5));
#6073=CARTESIAN_POINT('Origin',(9.2,4.3,1.6));
#6074=CARTESIAN_POINT('',(9.28902051504911,4.093359375,1.6));
#6075=CARTESIAN_POINT('',(9.11097948495089,4.093359375,1.6));
#6076=CARTESIAN_POINT('Origin',(9.2,3.5,1.6));
#6077=CARTESIAN_POINT('Origin',(9.2,4.3,1.6));
#6078=CARTESIAN_POINT('Origin',(9.2,4.3,0.9));
#6079=CARTESIAN_POINT('',(8.975,4.3,1.));
#6080=CARTESIAN_POINT('Origin',(9.2,4.3,1.));
#6081=CARTESIAN_POINT('',(8.975,4.3,1.5));
#6082=CARTESIAN_POINT('',(8.975,4.3,0.9));
#6083=CARTESIAN_POINT('',(9.11097948495089,4.093359375,1.5));
#6084=CARTESIAN_POINT('Origin',(9.2,4.3,1.5));
#6085=CARTESIAN_POINT('',(9.11097948495089,4.093359375,0.9));
#6086=CARTESIAN_POINT('',(9.28902051504911,4.093359375,1.5));
#6087=CARTESIAN_POINT('',(9.28902051504911,4.093359375,0.9));
#6088=CARTESIAN_POINT('Origin',(9.2,4.3,1.5));
#6089=CARTESIAN_POINT('Origin',(9.2,3.5,1.));
#6090=CARTESIAN_POINT('',(8.6,3.5,3.5));
#6091=CARTESIAN_POINT('Origin',(9.2,3.5,3.5));
#6092=CARTESIAN_POINT('',(8.6,3.5,1.5));
#6093=CARTESIAN_POINT('',(8.6,3.5,1.));
#6094=CARTESIAN_POINT('Origin',(9.2,3.5,1.5));
#6095=CARTESIAN_POINT('Origin',(9.2,3.5,1.5));
#6096=CARTESIAN_POINT('Origin',(9.2,3.5,1.5));
#6097=CARTESIAN_POINT('Origin',(9.2,3.5,1.5));
#6098=CARTESIAN_POINT('',(8.,3.5,1.5));
#6099=CARTESIAN_POINT('Origin',(9.2,3.5,1.5));
#6100=CARTESIAN_POINT('Origin',(9.2,3.5,1.));
#6101=CARTESIAN_POINT('',(8.,3.5,1.));
#6102=CARTESIAN_POINT('',(8.,3.5,1.));
#6103=CARTESIAN_POINT('Origin',(9.2,3.5,1.));
#6104=CARTESIAN_POINT('Origin',(9.2,3.5,3.5));
#6105=CARTESIAN_POINT('',(8.9,3.5,5.));
#6106=CARTESIAN_POINT('Origin',(9.2,3.5,5.));
#6107=CARTESIAN_POINT('',(8.9,3.5,3.5));
#6108=CARTESIAN_POINT('',(8.9,3.5,3.5));
#6109=CARTESIAN_POINT('Origin',(9.2,3.5,3.5));
#6110=CARTESIAN_POINT('Origin',(9.2,3.5,5.));
#6111=CARTESIAN_POINT('Origin',(9.2,3.5,3.5));
#6112=CARTESIAN_POINT('Origin',(9.2,3.5,1.));
#6113=CARTESIAN_POINT('',(0.,0.,0.));
#6114=CARTESIAN_POINT('Origin',(9.2,3.5,4.8));
#6115=CARTESIAN_POINT('',(8.895,3.5,5.));
#6116=CARTESIAN_POINT('Origin',(9.2,3.5,5.));
#6117=CARTESIAN_POINT('',(8.895,3.5,4.8));
#6118=CARTESIAN_POINT('',(8.895,3.5,4.8));
#6119=CARTESIAN_POINT('Origin',(9.2,3.5,4.8));
#6120=CARTESIAN_POINT('Origin',(9.2,3.5,4.8));
#6121=CARTESIAN_POINT('',(8.7,3.5,5.));
#6122=CARTESIAN_POINT('Origin',(9.2,3.5,5.));
#6123=CARTESIAN_POINT('',(8.7,3.5,4.8));
#6124=CARTESIAN_POINT('',(8.7,3.5,4.8));
#6125=CARTESIAN_POINT('Origin',(9.2,3.5,4.8));
#6126=CARTESIAN_POINT('Origin',(9.2,3.5,5.));
#6127=CARTESIAN_POINT('Origin',(9.2,3.5,4.8));
#6128=CARTESIAN_POINT('',(0.,0.,0.));
#6129=CARTESIAN_POINT('Origin',(9.2,3.5,5.));
#6130=CARTESIAN_POINT('',(8.975,3.5,5.2));
#6131=CARTESIAN_POINT('Origin',(9.2,3.5,5.2));
#6132=CARTESIAN_POINT('',(8.975,3.5,5.));
#6133=CARTESIAN_POINT('',(8.975,3.5,5.));
#6134=CARTESIAN_POINT('Origin',(9.2,3.5,5.));
#6135=CARTESIAN_POINT('Origin',(9.2,3.5,5.));
#6136=CARTESIAN_POINT('',(8.6,3.5,5.2));
#6137=CARTESIAN_POINT('Origin',(9.2,3.5,5.2));
#6138=CARTESIAN_POINT('',(8.6,3.5,5.));
#6139=CARTESIAN_POINT('',(8.6,3.5,5.));
#6140=CARTESIAN_POINT('Origin',(9.2,3.5,5.));
#6141=CARTESIAN_POINT('Origin',(9.2,3.5,5.2));
#6142=CARTESIAN_POINT('Origin',(9.2,3.5,5.));
#6143=CARTESIAN_POINT('',(0.,0.,0.));
#6144=CARTESIAN_POINT('Origin',(0.115470053837925,-0.5,-0.2));
#6145=CARTESIAN_POINT('',(0.23094010767585,-0.5,0.));
#6146=CARTESIAN_POINT('',(0.115470053837925,-0.5,-0.2));
#6147=CARTESIAN_POINT('',(0.23094010767585,-0.5,0.));
#6148=CARTESIAN_POINT('',(0.115470053837925,-0.8,-0.2));
#6149=CARTESIAN_POINT('',(0.115470053837925,-0.5,-0.2));
#6150=CARTESIAN_POINT('',(0.23094010767585,-0.8,0.));
#6151=CARTESIAN_POINT('',(0.23094010767585,-0.8,0.));
#6152=CARTESIAN_POINT('',(0.23094010767585,-0.5,0.));
#6153=CARTESIAN_POINT('Origin',(-0.115470053837925,-0.5,-0.2));
#6154=CARTESIAN_POINT('',(-0.115470053837925,-0.5,-0.2));
#6155=CARTESIAN_POINT('',(0.115470053837925,-0.5,-0.2));
#6156=CARTESIAN_POINT('',(-0.115470053837925,-0.8,-0.2));
#6157=CARTESIAN_POINT('',(-0.115470053837925,-0.5,-0.2));
#6158=CARTESIAN_POINT('',(0.115470053837925,-0.8,-0.2));
#6159=CARTESIAN_POINT('Origin',(-0.23094010767585,-0.5,-2.77555756156289E-17));
#6160=CARTESIAN_POINT('',(-0.23094010767585,-0.5,-2.82820063659975E-17));
#6161=CARTESIAN_POINT('',(-0.115470053837925,-0.5,-0.2));
#6162=CARTESIAN_POINT('',(-0.23094010767585,-0.8,-2.77555756156289E-17));
#6163=CARTESIAN_POINT('',(-0.23094010767585,-0.5,-2.82820063659975E-17));
#6164=CARTESIAN_POINT('',(-0.115470053837925,-0.8,-0.2));
#6165=CARTESIAN_POINT('Origin',(-0.115470053837925,-0.5,0.2));
#6166=CARTESIAN_POINT('',(-0.115470053837925,-0.5,0.2));
#6167=CARTESIAN_POINT('',(-0.23094010767585,-0.5,-2.82820063659975E-17));
#6168=CARTESIAN_POINT('',(-0.115470053837925,-0.8,0.2));
#6169=CARTESIAN_POINT('',(-0.115470053837925,-0.5,0.2));
#6170=CARTESIAN_POINT('',(-0.23094010767585,-0.8,-2.82820063659975E-17));
#6171=CARTESIAN_POINT('Origin',(0.115470053837925,-0.5,0.2));
#6172=CARTESIAN_POINT('',(0.115470053837925,-0.5,0.2));
#6173=CARTESIAN_POINT('',(-0.115470053837925,-0.5,0.2));
#6174=CARTESIAN_POINT('',(0.115470053837925,-0.8,0.2));
#6175=CARTESIAN_POINT('',(0.115470053837925,-0.5,0.2));
#6176=CARTESIAN_POINT('',(-0.115470053837925,-0.8,0.2));
#6177=CARTESIAN_POINT('Origin',(0.23094010767585,-0.5,0.));
#6178=CARTESIAN_POINT('',(0.115470053837925,-0.5,0.2));
#6179=CARTESIAN_POINT('',(0.115470053837925,-0.8,0.2));
#6180=CARTESIAN_POINT('Origin',(0.,-0.5,0.));
#6181=CARTESIAN_POINT('Origin',(0.,-0.8,0.));
#6182=CARTESIAN_POINT('Origin',(0.,-1.4,0.));
#6183=CARTESIAN_POINT('',(-0.24505,-1.4,3.00099698131059E-17));
#6184=CARTESIAN_POINT('Origin',(0.,-1.4,0.));
#6185=CARTESIAN_POINT('Origin',(0.375,0.5,0.));
#6186=CARTESIAN_POINT('',(-0.375,0.5,-4.59242549680257E-17));
#6187=CARTESIAN_POINT('Origin',(0.,0.5,0.));
#6188=CARTESIAN_POINT('Origin',(0.,0.475,0.));
#6189=CARTESIAN_POINT('',(-0.425,0.45,-5.20474889637625E-17));
#6190=CARTESIAN_POINT('Origin',(0.,0.45,0.));
#6191=CARTESIAN_POINT('',(-0.4,0.475,-4.89858719658941E-17));
#6192=CARTESIAN_POINT('Origin',(0.,0.24,0.));
#6193=CARTESIAN_POINT('',(-0.425,0.0299999999999998,-5.20474889637625E-17));
#6194=CARTESIAN_POINT('Origin',(0.,0.0299999999999998,0.));
#6195=CARTESIAN_POINT('',(-0.425,0.24,-5.20474889637625E-17));
#6196=CARTESIAN_POINT('Origin',(0.,0.0150000000000001,0.));
#6197=CARTESIAN_POINT('',(-0.395,4.85722573273506E-17,-4.83735485663204E-17));
#6198=CARTESIAN_POINT('Origin',(0.,0.,0.));
#6199=CARTESIAN_POINT('',(-0.41,0.0150000000000001,-5.02105187650415E-17));
#6200=CARTESIAN_POINT('Origin',(0.27,0.,0.));
#6201=CARTESIAN_POINT('',(-0.27,0.,-3.30654635769785E-17));
#6202=CARTESIAN_POINT('Origin',(0.,0.,0.));
#6203=CARTESIAN_POINT('Origin',(0.,-0.02,0.));
#6204=CARTESIAN_POINT('',(-0.24505,-0.0498999999999999,3.00099698131059E-17));
#6205=CARTESIAN_POINT('Origin',(0.,-0.0498999999999999,0.));
#6206=CARTESIAN_POINT('',(-0.26,-0.02,-3.18408167778312E-17));
#6207=CARTESIAN_POINT('Origin',(0.,-0.995,0.));
#6208=CARTESIAN_POINT('',(-0.24505,-0.995,-3.00099698131059E-17));
#6209=CARTESIAN_POINT('',(0.,0.,0.));
#6210=CARTESIAN_POINT('Origin',(0.0866025403784439,-0.4,-0.15));
#6211=CARTESIAN_POINT('',(0.173205080756888,-0.4,0.));
#6212=CARTESIAN_POINT('',(0.0866025403784439,-0.4,-0.15));
#6213=CARTESIAN_POINT('',(0.173205080756888,-0.4,0.));
#6214=CARTESIAN_POINT('',(0.0866025403784439,-0.64,-0.15));
#6215=CARTESIAN_POINT('',(0.0866025403784439,-0.4,-0.15));
#6216=CARTESIAN_POINT('',(0.173205080756888,-0.64,0.));
#6217=CARTESIAN_POINT('',(0.173205080756888,-0.64,0.));
#6218=CARTESIAN_POINT('',(0.173205080756888,-0.4,0.));
#6219=CARTESIAN_POINT('Origin',(-0.0866025403784438,-0.4,-0.15));
#6220=CARTESIAN_POINT('',(-0.0866025403784438,-0.4,-0.15));
#6221=CARTESIAN_POINT('',(0.0866025403784439,-0.4,-0.15));
#6222=CARTESIAN_POINT('',(-0.0866025403784438,-0.64,-0.15));
#6223=CARTESIAN_POINT('',(-0.0866025403784438,-0.4,-0.15));
#6224=CARTESIAN_POINT('',(0.0866025403784439,-0.64,-0.15));
#6225=CARTESIAN_POINT('Origin',(-0.173205080756888,-0.4,-2.77555756156289E-17));
#6226=CARTESIAN_POINT('',(-0.173205080756888,-0.4,-2.12115047744981E-17));
#6227=CARTESIAN_POINT('',(-0.0866025403784438,-0.4,-0.15));
#6228=CARTESIAN_POINT('',(-0.173205080756888,-0.64,-2.77555756156289E-17));
#6229=CARTESIAN_POINT('',(-0.173205080756888,-0.4,-2.12115047744981E-17));
#6230=CARTESIAN_POINT('',(-0.0866025403784438,-0.64,-0.15));
#6231=CARTESIAN_POINT('Origin',(-0.0866025403784439,-0.4,0.15));
#6232=CARTESIAN_POINT('',(-0.0866025403784439,-0.4,0.15));
#6233=CARTESIAN_POINT('',(-0.173205080756888,-0.4,-2.12115047744981E-17));
#6234=CARTESIAN_POINT('',(-0.0866025403784439,-0.64,0.15));
#6235=CARTESIAN_POINT('',(-0.0866025403784439,-0.4,0.15));
#6236=CARTESIAN_POINT('',(-0.173205080756888,-0.64,-2.12115047744981E-17));
#6237=CARTESIAN_POINT('Origin',(0.0866025403784439,-0.4,0.15));
#6238=CARTESIAN_POINT('',(0.0866025403784439,-0.4,0.15));
#6239=CARTESIAN_POINT('',(-0.0866025403784439,-0.4,0.15));
#6240=CARTESIAN_POINT('',(0.0866025403784439,-0.64,0.15));
#6241=CARTESIAN_POINT('',(0.0866025403784439,-0.4,0.15));
#6242=CARTESIAN_POINT('',(-0.0866025403784439,-0.64,0.15));
#6243=CARTESIAN_POINT('Origin',(0.173205080756888,-0.4,0.));
#6244=CARTESIAN_POINT('',(0.0866025403784439,-0.4,0.15));
#6245=CARTESIAN_POINT('',(0.0866025403784439,-0.64,0.15));
#6246=CARTESIAN_POINT('Origin',(0.,-0.4,-2.77555756156289E-17));
#6247=CARTESIAN_POINT('Origin',(0.,-0.64,-2.77555756156289E-17));
#6248=CARTESIAN_POINT('Origin',(0.,-1.,0.));
#6249=CARTESIAN_POINT('',(-0.1954,-1.,2.39295984553393E-17));
#6250=CARTESIAN_POINT('Origin',(0.,-1.,0.));
#6251=CARTESIAN_POINT('Origin',(0.3,0.4,0.));
#6252=CARTESIAN_POINT('',(-0.3,0.4,-3.67394039744206E-17));
#6253=CARTESIAN_POINT('Origin',(0.,0.4,0.));
#6254=CARTESIAN_POINT('Origin',(0.,0.375,0.));
#6255=CARTESIAN_POINT('',(-0.35,0.35,-4.28626379701573E-17));
#6256=CARTESIAN_POINT('Origin',(0.,0.35,0.));
#6257=CARTESIAN_POINT('',(-0.325,0.375,-3.9801020972289E-17));
#6258=CARTESIAN_POINT('Origin',(0.,0.19,0.));
#6259=CARTESIAN_POINT('',(-0.35,0.03,-4.28626379701574E-17));
#6260=CARTESIAN_POINT('Origin',(0.,0.03,0.));
#6261=CARTESIAN_POINT('',(-0.35,0.19,-4.28626379701574E-17));
#6262=CARTESIAN_POINT('Origin',(0.,0.0149999999999999,0.));
#6263=CARTESIAN_POINT('',(-0.32,-3.29597460435593E-17,-3.91886975727153E-17));
#6264=CARTESIAN_POINT('Origin',(0.,0.,0.));
#6265=CARTESIAN_POINT('',(-0.335,0.0149999999999999,-4.10256677714363E-17));
#6266=CARTESIAN_POINT('Origin',(0.22,0.,0.));
#6267=CARTESIAN_POINT('',(-0.22,-6.93889390390723E-18,-2.69422295812418E-17));
#6268=CARTESIAN_POINT('Origin',(0.,0.,0.));
#6269=CARTESIAN_POINT('Origin',(0.,-0.02,0.));
#6270=CARTESIAN_POINT('',(-0.1954,-0.0492,2.39295984553393E-17));
#6271=CARTESIAN_POINT('Origin',(0.,-0.0492,0.));
#6272=CARTESIAN_POINT('',(-0.21,-0.02,-2.57175827820944E-17));
#6273=CARTESIAN_POINT('Origin',(0.,-0.8,0.));
#6274=CARTESIAN_POINT('',(-0.1954,-0.8,-2.39295984553393E-17));
#6275=CARTESIAN_POINT('',(0.,0.,0.));
#6276=CARTESIAN_POINT('',(0.,0.,0.));
#6277=CARTESIAN_POINT('',(0.,0.,0.));
#6278=CARTESIAN_POINT('',(0.,0.,0.));
#6279=CARTESIAN_POINT('',(0.,0.,0.));
#6280=CARTESIAN_POINT('',(0.,0.,0.));
#6281=CARTESIAN_POINT('',(0.,0.,0.));
#6282=CARTESIAN_POINT('',(0.,0.,0.));
#6283=CARTESIAN_POINT('',(0.,0.,0.));
#6284=CARTESIAN_POINT('',(0.,0.,0.));
#6285=CARTESIAN_POINT('',(0.,0.,0.));
#6286=CARTESIAN_POINT('',(0.,0.,0.));
#6287=CARTESIAN_POINT('',(0.,0.,0.));
#6288=CARTESIAN_POINT('',(0.,0.,0.));
#6289=CARTESIAN_POINT('',(0.,0.,0.));
#6290=CARTESIAN_POINT('',(-3.5,-1.8,1.8));
#6291=CARTESIAN_POINT('',(-3.5,1.8,1.8));
#6292=CARTESIAN_POINT('',(3.5,-1.8,1.8));
#6293=CARTESIAN_POINT('',(3.5,1.8,1.8));
#6294=CARTESIAN_POINT('',(-6.5,-6.5,1.8));
#6295=CARTESIAN_POINT('',(-6.5,-4.2,1.8));
#6296=CARTESIAN_POINT('',(6.5,-6.5,1.8));
#6297=CARTESIAN_POINT('',(6.5,-4.2,1.8));
#6298=CARTESIAN_POINT('',(-7.8,-6.,3.5));
#6299=CARTESIAN_POINT('',(7.8,-6.,3.5));
#6300=CARTESIAN_POINT('',(9.2,2.7,1.5));
#6301=CARTESIAN_POINT('',(9.2,4.3,1.5));
#6302=CARTESIAN_POINT('',(9.2,3.5,5.2));
#6303=CARTESIAN_POINT('',(0.,0.,0.));
#6304=CARTESIAN_POINT('',(0.,0.,0.));
#6305=CARTESIAN_POINT('Origin',(2.,1.,3.4));
#6306=CARTESIAN_POINT('',(1.3,1.,3.5));
#6307=CARTESIAN_POINT('Origin',(2.,1.,3.5));
#6308=CARTESIAN_POINT('',(1.3,1.,4.5));
#6309=CARTESIAN_POINT('',(1.3,1.,3.4));
#6310=CARTESIAN_POINT('Origin',(2.,1.,4.5));
#6311=CARTESIAN_POINT('Origin',(2.,-1.,3.4));
#6312=CARTESIAN_POINT('',(1.3,-1.,3.5));
#6313=CARTESIAN_POINT('Origin',(2.,-1.,3.5));
#6314=CARTESIAN_POINT('',(1.3,-1.,4.5));
#6315=CARTESIAN_POINT('',(1.3,-1.,3.4));
#6316=CARTESIAN_POINT('Origin',(2.,-1.,4.5));
#6317=CARTESIAN_POINT('Origin',(-2.,1.,3.4));
#6318=CARTESIAN_POINT('',(-2.6,1.,3.5));
#6319=CARTESIAN_POINT('Origin',(-2.,1.,3.5));
#6320=CARTESIAN_POINT('',(-2.6,1.,4.5));
#6321=CARTESIAN_POINT('',(-2.6,1.,3.4));
#6322=CARTESIAN_POINT('Origin',(-2.,1.,4.5));
#6323=CARTESIAN_POINT('Origin',(-2.,-1.,3.4));
#6324=CARTESIAN_POINT('',(-2.6,-1.,3.5));
#6325=CARTESIAN_POINT('Origin',(-2.,-1.,3.5));
#6326=CARTESIAN_POINT('',(-2.6,-1.,4.5));
#6327=CARTESIAN_POINT('',(-2.6,-1.,3.4));
#6328=CARTESIAN_POINT('Origin',(-2.,-1.,4.5));
#6329=CARTESIAN_POINT('Origin',(-5.5,-6.,3.5));
#6330=CARTESIAN_POINT('',(-5.5,-6.,4.3));
#6331=CARTESIAN_POINT('',(-5.5,-5.2,3.5));
#6332=CARTESIAN_POINT('Origin',(-5.5,-6.,3.5));
#6333=CARTESIAN_POINT('',(-5.5,-5.,4.3));
#6334=CARTESIAN_POINT('',(-5.5,-4.5,4.3));
#6335=CARTESIAN_POINT('',(-5.5,-5.,3.5));
#6336=CARTESIAN_POINT('',(-5.5,-5.,3.7));
#6337=CARTESIAN_POINT('',(-5.5,-6.,3.5));
#6338=CARTESIAN_POINT('',(-5.5,-6.,3.905));
#6339=CARTESIAN_POINT('Origin',(-5.5,-6.,3.5));
#6340=CARTESIAN_POINT('Origin',(-5.5,-4.5,4.3));
#6341=CARTESIAN_POINT('',(5.5,-5.,4.3));
#6342=CARTESIAN_POINT('',(-6.75,-5.,4.3));
#6343=CARTESIAN_POINT('',(5.5,-6.,4.3));
#6344=CARTESIAN_POINT('',(-5.5,-6.,4.3));
#6345=CARTESIAN_POINT('',(5.5,-4.5,4.3));
#6346=CARTESIAN_POINT('Origin',(5.5,-6.,3.5));
#6347=CARTESIAN_POINT('',(5.5,-5.2,3.5));
#6348=CARTESIAN_POINT('Origin',(5.5,-6.,3.5));
#6349=CARTESIAN_POINT('',(5.5,-5.,3.5));
#6350=CARTESIAN_POINT('',(5.5,-6.,3.5));
#6351=CARTESIAN_POINT('',(5.5,-5.,3.7));
#6352=CARTESIAN_POINT('',(5.5,-6.,3.905));
#6353=CARTESIAN_POINT('Origin',(5.5,-6.,3.5));
#6354=CARTESIAN_POINT('Origin',(-5.5,-6.,3.5));
#6355=CARTESIAN_POINT('',(-5.5,-6.,3.905));
#6356=CARTESIAN_POINT('Origin',(-5.5,-6.,3.5));
#6357=CARTESIAN_POINT('',(-5.5,-5.2,3.5));
#6358=CARTESIAN_POINT('Origin',(-8.,-5.,3.5));
#6359=CARTESIAN_POINT('',(5.9,-5.,3.5));
#6360=CARTESIAN_POINT('',(-8.,-5.,3.5));
#6361=CARTESIAN_POINT('',(5.9,-5.,4.5));
#6362=CARTESIAN_POINT('',(5.9,-5.,3.45));
#6363=CARTESIAN_POINT('',(-5.9,-5.,4.5));
#6364=CARTESIAN_POINT('',(-8.,-5.,4.5));
#6365=CARTESIAN_POINT('',(-5.9,-5.,3.5));
#6366=CARTESIAN_POINT('',(-5.9,-5.,3.45));
#6367=CARTESIAN_POINT('',(-8.,-5.,3.5));
#6368=CARTESIAN_POINT('Origin',(5.9,-3.5,3.4));
#6369=CARTESIAN_POINT('',(5.9,-3.5,3.5));
#6370=CARTESIAN_POINT('',(5.9,-1.75,3.5));
#6371=CARTESIAN_POINT('',(5.9,-3.5,4.5));
#6372=CARTESIAN_POINT('',(5.9,-3.5,3.4));
#6373=CARTESIAN_POINT('',(5.9,-1.75,4.5));
#6374=CARTESIAN_POINT('Origin',(7.1,-3.5,3.4));
#6375=CARTESIAN_POINT('',(7.1,-3.5,3.5));
#6376=CARTESIAN_POINT('',(3.55,-3.5,3.5));
#6377=CARTESIAN_POINT('',(7.1,-3.5,4.5));
#6378=CARTESIAN_POINT('',(7.1,-3.5,3.4));
#6379=CARTESIAN_POINT('',(3.55,-3.5,4.5));
#6380=CARTESIAN_POINT('Origin',(7.1,-5.1,3.4));
#6381=CARTESIAN_POINT('',(7.1,-5.,3.5));
#6382=CARTESIAN_POINT('',(7.1,-2.55,3.5));
#6383=CARTESIAN_POINT('',(7.1,-5.,4.5));
#6384=CARTESIAN_POINT('',(7.1,-5.,3.45));
#6385=CARTESIAN_POINT('',(7.1,-2.55,4.5));
#6386=CARTESIAN_POINT('Origin',(0.,0.,3.5));
#6387=CARTESIAN_POINT('',(-5.9,-3.5,3.5));
#6388=CARTESIAN_POINT('',(-5.9,-2.55,3.5));
#6389=CARTESIAN_POINT('',(-7.1,-3.5,3.5));
#6390=CARTESIAN_POINT('',(-2.95,-3.5,3.5));
#6391=CARTESIAN_POINT('',(-7.1,-5.,3.5));
#6392=CARTESIAN_POINT('',(-7.1,-1.75,3.5));
#6393=CARTESIAN_POINT('',(-8.,-5.,3.5));
#6394=CARTESIAN_POINT('',(-8.,-5.,3.5));
#6395=CARTESIAN_POINT('',(-8.,5.,3.5));
#6396=CARTESIAN_POINT('',(-8.,5.,3.5));
#6397=CARTESIAN_POINT('',(8.,5.,3.5));
#6398=CARTESIAN_POINT('',(8.,5.,3.5));
#6399=CARTESIAN_POINT('',(8.,-5.,3.5));
#6400=CARTESIAN_POINT('',(8.,-5.,3.5));
#6401=CARTESIAN_POINT('',(-8.,-5.,3.5));
#6402=CARTESIAN_POINT('Origin',(-5.9,-5.1,3.4));
#6403=CARTESIAN_POINT('',(-5.9,-3.5,4.5));
#6404=CARTESIAN_POINT('',(-5.9,-2.55,4.5));
#6405=CARTESIAN_POINT('',(-5.9,-3.5,3.4));
#6406=CARTESIAN_POINT('Origin',(-5.9,-3.5,3.4));
#6407=CARTESIAN_POINT('',(-7.1,-3.5,4.5));
#6408=CARTESIAN_POINT('',(-2.95,-3.5,4.5));
#6409=CARTESIAN_POINT('',(-7.1,-3.5,3.4));
#6410=CARTESIAN_POINT('Origin',(-7.1,-3.5,3.4));
#6411=CARTESIAN_POINT('',(-7.1,-5.,4.5));
#6412=CARTESIAN_POINT('',(-7.1,-1.75,4.5));
#6413=CARTESIAN_POINT('',(-7.1,-5.,3.45));
#6414=CARTESIAN_POINT('Origin',(-8.,-5.,3.5));
#6415=CARTESIAN_POINT('',(-8.,-5.,4.5));
#6416=CARTESIAN_POINT('',(-8.,-5.,4.5));
#6417=CARTESIAN_POINT('',(-8.,-5.,3.5));
#6418=CARTESIAN_POINT('Origin',(-8.,-5.,3.5));
#6419=CARTESIAN_POINT('',(8.,-5.,4.5));
#6420=CARTESIAN_POINT('',(8.,-5.,3.5));
#6421=CARTESIAN_POINT('',(-8.,-5.,4.5));
#6422=CARTESIAN_POINT('Origin',(8.,5.,3.5));
#6423=CARTESIAN_POINT('',(-8.,5.,4.5));
#6424=CARTESIAN_POINT('',(-8.,5.,3.5));
#6425=CARTESIAN_POINT('',(8.,5.,4.5));
#6426=CARTESIAN_POINT('',(8.,5.,4.5));
#6427=CARTESIAN_POINT('',(8.,5.,3.5));
#6428=CARTESIAN_POINT('Origin',(8.,-5.,3.5));
#6429=CARTESIAN_POINT('',(8.,-5.,4.5));
#6430=CARTESIAN_POINT('Origin',(-8.,5.,3.5));
#6431=CARTESIAN_POINT('',(-8.,5.,4.5));
#6432=CARTESIAN_POINT('Origin',(0.,0.,4.5));
#6433=CARTESIAN_POINT('',(0.,0.,0.));
#6434=CARTESIAN_POINT('Origin',(-2.,-1.,4.5));
#6435=CARTESIAN_POINT('',(-2.8,-1.,4.5));
#6436=CARTESIAN_POINT('Origin',(-2.,-1.,4.5));
#6437=CARTESIAN_POINT('',(-2.6,-1.,4.5));
#6438=CARTESIAN_POINT('Origin',(-2.,-1.,4.5));
#6439=CARTESIAN_POINT('Origin',(-2.,-1.,4.5));
#6440=CARTESIAN_POINT('',(-2.8,-1.,4.7));
#6441=CARTESIAN_POINT('Origin',(-2.,-1.,4.7));
#6442=CARTESIAN_POINT('',(-2.8,-1.,4.5));
#6443=CARTESIAN_POINT('Origin',(-2.,-1.,4.7));
#6444=CARTESIAN_POINT('',(-2.4,-1.,4.7));
#6445=CARTESIAN_POINT('Origin',(-2.,-1.,4.7));
#6446=CARTESIAN_POINT('Origin',(-2.,-1.,2.5));
#6447=CARTESIAN_POINT('',(-2.4,-1.,2.5));
#6448=CARTESIAN_POINT('',(-2.4,-1.,2.5));
#6449=CARTESIAN_POINT('Origin',(-2.,-1.,2.5));
#6450=CARTESIAN_POINT('Origin',(-2.,-1.,2.5));
#6451=CARTESIAN_POINT('',(-2.6,-1.,2.5));
#6452=CARTESIAN_POINT('',(-2.6,-1.,2.5));
#6453=CARTESIAN_POINT('Origin',(-2.,-1.,2.5));
#6454=CARTESIAN_POINT('Origin',(-2.,-1.,2.5));
#6455=CARTESIAN_POINT('',(0.,0.,0.));
#6456=CARTESIAN_POINT('Origin',(-2.,1.,4.5));
#6457=CARTESIAN_POINT('',(-2.8,1.,4.5));
#6458=CARTESIAN_POINT('Origin',(-2.,1.,4.5));
#6459=CARTESIAN_POINT('',(-2.6,1.,4.5));
#6460=CARTESIAN_POINT('Origin',(-2.,1.,4.5));
#6461=CARTESIAN_POINT('Origin',(-2.,1.,4.5));
#6462=CARTESIAN_POINT('',(-2.8,1.,4.7));
#6463=CARTESIAN_POINT('Origin',(-2.,1.,4.7));
#6464=CARTESIAN_POINT('',(-2.8,1.,4.5));
#6465=CARTESIAN_POINT('Origin',(-2.,1.,4.7));
#6466=CARTESIAN_POINT('',(-2.4,1.,4.7));
#6467=CARTESIAN_POINT('Origin',(-2.,1.,4.7));
#6468=CARTESIAN_POINT('Origin',(-2.,1.,2.5));
#6469=CARTESIAN_POINT('',(-2.4,1.,2.5));
#6470=CARTESIAN_POINT('',(-2.4,1.,2.5));
#6471=CARTESIAN_POINT('Origin',(-2.,1.,2.5));
#6472=CARTESIAN_POINT('Origin',(-2.,1.,2.5));
#6473=CARTESIAN_POINT('',(-2.6,1.,2.5));
#6474=CARTESIAN_POINT('',(-2.6,1.,2.5));
#6475=CARTESIAN_POINT('Origin',(-2.,1.,2.5));
#6476=CARTESIAN_POINT('Origin',(-2.,1.,2.5));
#6477=CARTESIAN_POINT('',(0.,0.,0.));
#6478=CARTESIAN_POINT('Origin',(2.,-1.,4.5));
#6479=CARTESIAN_POINT('',(1.1,-1.,4.5));
#6480=CARTESIAN_POINT('Origin',(2.,-1.,4.5));
#6481=CARTESIAN_POINT('',(1.3,-1.,4.5));
#6482=CARTESIAN_POINT('Origin',(2.,-1.,4.5));
#6483=CARTESIAN_POINT('Origin',(2.,-1.,4.5));
#6484=CARTESIAN_POINT('',(1.1,-1.,4.7));
#6485=CARTESIAN_POINT('Origin',(2.,-1.,4.7));
#6486=CARTESIAN_POINT('',(1.1,-1.,4.5));
#6487=CARTESIAN_POINT('Origin',(2.,-1.,4.7));
#6488=CARTESIAN_POINT('',(1.5,-1.,4.7));
#6489=CARTESIAN_POINT('Origin',(2.,-1.,4.7));
#6490=CARTESIAN_POINT('Origin',(2.,-1.,2.5));
#6491=CARTESIAN_POINT('',(1.5,-1.,2.5));
#6492=CARTESIAN_POINT('',(1.5,-1.,2.5));
#6493=CARTESIAN_POINT('Origin',(2.,-1.,2.5));
#6494=CARTESIAN_POINT('Origin',(2.,-1.,2.5));
#6495=CARTESIAN_POINT('',(1.3,-1.,2.5));
#6496=CARTESIAN_POINT('',(1.3,-1.,2.5));
#6497=CARTESIAN_POINT('Origin',(2.,-1.,2.5));
#6498=CARTESIAN_POINT('Origin',(2.,-1.,2.5));
#6499=CARTESIAN_POINT('',(0.,0.,0.));
#6500=CARTESIAN_POINT('Origin',(2.,1.,4.5));
#6501=CARTESIAN_POINT('',(1.1,1.,4.5));
#6502=CARTESIAN_POINT('Origin',(2.,1.,4.5));
#6503=CARTESIAN_POINT('',(1.3,1.,4.5));
#6504=CARTESIAN_POINT('Origin',(2.,1.,4.5));
#6505=CARTESIAN_POINT('Origin',(2.,1.,4.5));
#6506=CARTESIAN_POINT('',(1.1,1.,4.7));
#6507=CARTESIAN_POINT('Origin',(2.,1.,4.7));
#6508=CARTESIAN_POINT('',(1.1,1.,4.5));
#6509=CARTESIAN_POINT('Origin',(2.,1.,4.7));
#6510=CARTESIAN_POINT('',(1.5,1.,4.7));
#6511=CARTESIAN_POINT('Origin',(2.,1.,4.7));
#6512=CARTESIAN_POINT('Origin',(2.,1.,2.5));
#6513=CARTESIAN_POINT('',(1.5,1.,2.5));
#6514=CARTESIAN_POINT('',(1.5,1.,2.5));
#6515=CARTESIAN_POINT('Origin',(2.,1.,2.5));
#6516=CARTESIAN_POINT('Origin',(2.,1.,2.5));
#6517=CARTESIAN_POINT('',(1.3,1.,2.5));
#6518=CARTESIAN_POINT('',(1.3,1.,2.5));
#6519=CARTESIAN_POINT('Origin',(2.,1.,2.5));
#6520=CARTESIAN_POINT('Origin',(2.,1.,2.5));
#6521=CARTESIAN_POINT('',(0.,0.,0.));
#6522=CARTESIAN_POINT('',(0.,0.,0.));
#6523=CARTESIAN_POINT('',(0.,0.,0.));
#6524=CARTESIAN_POINT('',(0.,0.,0.));
#6525=CARTESIAN_POINT('',(0.,0.,0.));
#6526=CARTESIAN_POINT('',(0.,0.,0.));
#6527=CARTESIAN_POINT('',(0.,0.,0.));
#6528=CARTESIAN_POINT('Origin',(9.2,3.5,3.4));
#6529=CARTESIAN_POINT('',(8.895,3.5,3.5));
#6530=CARTESIAN_POINT('Origin',(9.2,3.5,3.5));
#6531=CARTESIAN_POINT('',(8.895,3.5,4.8));
#6532=CARTESIAN_POINT('',(8.895,3.5,3.4));
#6533=CARTESIAN_POINT('Origin',(9.2,3.5,4.8));
#6534=CARTESIAN_POINT('Origin',(9.6,3.5,4.5));
#6535=CARTESIAN_POINT('',(9.6,4.76491106406735,4.5));
#6536=CARTESIAN_POINT('',(9.6,4.76491106406735,4.8));
#6537=CARTESIAN_POINT('',(9.6,4.76491106406735,4.5));
#6538=CARTESIAN_POINT('',(9.6,7.5,4.5));
#6539=CARTESIAN_POINT('',(9.6,3.5,4.5));
#6540=CARTESIAN_POINT('',(9.6,7.5,4.8));
#6541=CARTESIAN_POINT('',(9.6,7.5,4.5));
#6542=CARTESIAN_POINT('',(9.6,3.5,4.8));
#6543=CARTESIAN_POINT('Origin',(9.6,7.5,4.5));
#6544=CARTESIAN_POINT('',(8.8,7.5,4.5));
#6545=CARTESIAN_POINT('',(9.6,7.5,4.5));
#6546=CARTESIAN_POINT('',(8.8,7.5,4.8));
#6547=CARTESIAN_POINT('',(8.8,7.5,4.5));
#6548=CARTESIAN_POINT('',(9.6,7.5,4.8));
#6549=CARTESIAN_POINT('Origin',(8.8,7.5,4.5));
#6550=CARTESIAN_POINT('',(8.8,4.8856406460551,4.8));
#6551=CARTESIAN_POINT('',(8.8,4.8856406460551,4.5));
#6552=CARTESIAN_POINT('',(8.8,4.8856406460551,4.5));
#6553=CARTESIAN_POINT('',(8.8,7.5,4.8));
#6554=CARTESIAN_POINT('',(8.8,7.5,4.5));
#6555=CARTESIAN_POINT('Origin',(9.,3.5,4.8));
#6556=CARTESIAN_POINT('Origin',(9.,3.5,4.8));
#6557=CARTESIAN_POINT('Origin',(9.,3.5,4.5));
#6558=CARTESIAN_POINT('Origin',(9.,3.5,4.5));
#6559=CARTESIAN_POINT('',(8.,3.5,4.5));
#6560=CARTESIAN_POINT('Origin',(9.,3.5,4.5));
#6561=CARTESIAN_POINT('Origin',(9.,3.5,4.5));
#6562=CARTESIAN_POINT('Origin',(9.,3.5,3.5));
#6563=CARTESIAN_POINT('',(8.,3.5,3.5));
#6564=CARTESIAN_POINT('',(8.,3.5,3.5));
#6565=CARTESIAN_POINT('Origin',(9.,3.5,3.5));
#6566=CARTESIAN_POINT('Origin',(9.,3.5,3.5));
#6567=CARTESIAN_POINT('',(0.,0.,0.));
#6568=CARTESIAN_POINT('Origin',(9.2,7.5,4.8));
#6569=CARTESIAN_POINT('',(8.6,7.5,6.3));
#6570=CARTESIAN_POINT('Origin',(9.2,7.5,6.3));
#6571=CARTESIAN_POINT('',(8.6,7.5,4.8));
#6572=CARTESIAN_POINT('',(8.6,7.5,4.8));
#6573=CARTESIAN_POINT('Origin',(9.2,7.5,4.8));
#6574=CARTESIAN_POINT('Origin',(9.2,7.5,6.3));
#6575=CARTESIAN_POINT('Origin',(9.2,7.5,4.8));
#6576=CARTESIAN_POINT('',(0.,0.,0.));
#6577=CARTESIAN_POINT('',(0.,0.,0.));
#6578=CARTESIAN_POINT('',(0.,0.,0.));
#6579=CARTESIAN_POINT('',(0.,0.,0.));
#6580=CARTESIAN_POINT('',(0.,0.,0.));
#6581=UNCERTAINTY_MEASURE_WITH_UNIT(LENGTH_MEASURE(0.001),#6639,
'DISTANCE_ACCURACY_VALUE',
'Maximum model space distance between geometric entities at asserted c
onnectivities');
#6582=UNCERTAINTY_MEASURE_WITH_UNIT(LENGTH_MEASURE(0.001),#6639,
'DISTANCE_ACCURACY_VALUE',
'Maximum model space distance between geometric entities at asserted c
onnectivities');
#6583=UNCERTAINTY_MEASURE_WITH_UNIT(LENGTH_MEASURE(0.001),#6639,
'DISTANCE_ACCURACY_VALUE',
'Maximum model space distance between geometric entities at asserted c
onnectivities');
#6584=UNCERTAINTY_MEASURE_WITH_UNIT(LENGTH_MEASURE(0.001),#6639,
'DISTANCE_ACCURACY_VALUE',
'Maximum model space distance between geometric entities at asserted c
onnectivities');
#6585=UNCERTAINTY_MEASURE_WITH_UNIT(LENGTH_MEASURE(0.001),#6639,
'DISTANCE_ACCURACY_VALUE',
'Maximum model space distance between geometric entities at asserted c
onnectivities');
#6586=UNCERTAINTY_MEASURE_WITH_UNIT(LENGTH_MEASURE(0.001),#6639,
'DISTANCE_ACCURACY_VALUE',
'Maximum model space distance between geometric entities at asserted c
onnectivities');
#6587=UNCERTAINTY_MEASURE_WITH_UNIT(LENGTH_MEASURE(0.001),#6639,
'DISTANCE_ACCURACY_VALUE',
'Maximum model space distance between geometric entities at asserted c
onnectivities');
#6588=UNCERTAINTY_MEASURE_WITH_UNIT(LENGTH_MEASURE(0.001),#6639,
'DISTANCE_ACCURACY_VALUE',
'Maximum model space distance between geometric entities at asserted c
onnectivities');
#6589=UNCERTAINTY_MEASURE_WITH_UNIT(LENGTH_MEASURE(0.001),#6639,
'DISTANCE_ACCURACY_VALUE',
'Maximum model space distance between geometric entities at asserted c
onnectivities');
#6590=UNCERTAINTY_MEASURE_WITH_UNIT(LENGTH_MEASURE(0.001),#6639,
'DISTANCE_ACCURACY_VALUE',
'Maximum model space distance between geometric entities at asserted c
onnectivities');
#6591=UNCERTAINTY_MEASURE_WITH_UNIT(LENGTH_MEASURE(0.001),#6639,
'DISTANCE_ACCURACY_VALUE',
'Maximum model space distance between geometric entities at asserted c
onnectivities');
#6592=UNCERTAINTY_MEASURE_WITH_UNIT(LENGTH_MEASURE(0.001),#6639,
'DISTANCE_ACCURACY_VALUE',
'Maximum model space distance between geometric entities at asserted c
onnectivities');
#6593=UNCERTAINTY_MEASURE_WITH_UNIT(LENGTH_MEASURE(0.001),#6639,
'DISTANCE_ACCURACY_VALUE',
'Maximum model space distance between geometric entities at asserted c
onnectivities');
#6594=UNCERTAINTY_MEASURE_WITH_UNIT(LENGTH_MEASURE(0.001),#6639,
'DISTANCE_ACCURACY_VALUE',
'Maximum model space distance between geometric entities at asserted c
onnectivities');
#6595=UNCERTAINTY_MEASURE_WITH_UNIT(LENGTH_MEASURE(0.001),#6639,
'DISTANCE_ACCURACY_VALUE',
'Maximum model space distance between geometric entities at asserted c
onnectivities');
#6596=UNCERTAINTY_MEASURE_WITH_UNIT(LENGTH_MEASURE(0.001),#6639,
'DISTANCE_ACCURACY_VALUE',
'Maximum model space distance between geometric entities at asserted c
onnectivities');
#6597=UNCERTAINTY_MEASURE_WITH_UNIT(LENGTH_MEASURE(0.001),#6639,
'DISTANCE_ACCURACY_VALUE',
'Maximum model space distance between geometric entities at asserted c
onnectivities');
#6598=UNCERTAINTY_MEASURE_WITH_UNIT(LENGTH_MEASURE(0.001),#6639,
'DISTANCE_ACCURACY_VALUE',
'Maximum model space distance between geometric entities at asserted c
onnectivities');
#6599=UNCERTAINTY_MEASURE_WITH_UNIT(LENGTH_MEASURE(0.001),#6639,
'DISTANCE_ACCURACY_VALUE',
'Maximum model space distance between geometric entities at asserted c
onnectivities');
#6600=UNCERTAINTY_MEASURE_WITH_UNIT(LENGTH_MEASURE(0.001),#6639,
'DISTANCE_ACCURACY_VALUE',
'Maximum model space distance between geometric entities at asserted c
onnectivities');
#6601=UNCERTAINTY_MEASURE_WITH_UNIT(LENGTH_MEASURE(0.001),#6639,
'DISTANCE_ACCURACY_VALUE',
'Maximum model space distance between geometric entities at asserted c
onnectivities');
#6602=UNCERTAINTY_MEASURE_WITH_UNIT(LENGTH_MEASURE(0.001),#6639,
'DISTANCE_ACCURACY_VALUE',
'Maximum model space distance between geometric entities at asserted c
onnectivities');
#6603=UNCERTAINTY_MEASURE_WITH_UNIT(LENGTH_MEASURE(0.001),#6639,
'DISTANCE_ACCURACY_VALUE',
'Maximum model space distance between geometric entities at asserted c
onnectivities');
#6604=UNCERTAINTY_MEASURE_WITH_UNIT(LENGTH_MEASURE(0.001),#6639,
'DISTANCE_ACCURACY_VALUE',
'Maximum model space distance between geometric entities at asserted c
onnectivities');
#6605=UNCERTAINTY_MEASURE_WITH_UNIT(LENGTH_MEASURE(0.001),#6639,
'DISTANCE_ACCURACY_VALUE',
'Maximum model space distance between geometric entities at asserted c
onnectivities');
#6606=UNCERTAINTY_MEASURE_WITH_UNIT(LENGTH_MEASURE(0.001),#6639,
'DISTANCE_ACCURACY_VALUE',
'Maximum model space distance between geometric entities at asserted c
onnectivities');
#6607=UNCERTAINTY_MEASURE_WITH_UNIT(LENGTH_MEASURE(0.001),#6639,
'DISTANCE_ACCURACY_VALUE',
'Maximum model space distance between geometric entities at asserted c
onnectivities');
#6608=UNCERTAINTY_MEASURE_WITH_UNIT(LENGTH_MEASURE(0.001),#6639,
'DISTANCE_ACCURACY_VALUE',
'Maximum model space distance between geometric entities at asserted c
onnectivities');
#6609=UNCERTAINTY_MEASURE_WITH_UNIT(LENGTH_MEASURE(0.001),#6639,
'DISTANCE_ACCURACY_VALUE',
'Maximum model space distance between geometric entities at asserted c
onnectivities');
#6610=(
GEOMETRIC_REPRESENTATION_CONTEXT(3)
GLOBAL_UNCERTAINTY_ASSIGNED_CONTEXT((#6581))
GLOBAL_UNIT_ASSIGNED_CONTEXT((#6639,#6641,#6642))
REPRESENTATION_CONTEXT('','3D')
);
#6611=(
GEOMETRIC_REPRESENTATION_CONTEXT(3)
GLOBAL_UNCERTAINTY_ASSIGNED_CONTEXT((#6582))
GLOBAL_UNIT_ASSIGNED_CONTEXT((#6639,#6641,#6642))
REPRESENTATION_CONTEXT('','3D')
);
#6612=(
GEOMETRIC_REPRESENTATION_CONTEXT(3)
GLOBAL_UNCERTAINTY_ASSIGNED_CONTEXT((#6583))
GLOBAL_UNIT_ASSIGNED_CONTEXT((#6639,#6641,#6642))
REPRESENTATION_CONTEXT('','3D')
);
#6613=(
GEOMETRIC_REPRESENTATION_CONTEXT(3)
GLOBAL_UNCERTAINTY_ASSIGNED_CONTEXT((#6584))
GLOBAL_UNIT_ASSIGNED_CONTEXT((#6639,#6641,#6642))
REPRESENTATION_CONTEXT('','3D')
);
#6614=(
GEOMETRIC_REPRESENTATION_CONTEXT(3)
GLOBAL_UNCERTAINTY_ASSIGNED_CONTEXT((#6585))
GLOBAL_UNIT_ASSIGNED_CONTEXT((#6639,#6641,#6642))
REPRESENTATION_CONTEXT('','3D')
);
#6615=(
GEOMETRIC_REPRESENTATION_CONTEXT(3)
GLOBAL_UNCERTAINTY_ASSIGNED_CONTEXT((#6586))
GLOBAL_UNIT_ASSIGNED_CONTEXT((#6639,#6641,#6642))
REPRESENTATION_CONTEXT('','3D')
);
#6616=(
GEOMETRIC_REPRESENTATION_CONTEXT(3)
GLOBAL_UNCERTAINTY_ASSIGNED_CONTEXT((#6587))
GLOBAL_UNIT_ASSIGNED_CONTEXT((#6639,#6641,#6642))
REPRESENTATION_CONTEXT('','3D')
);
#6617=(
GEOMETRIC_REPRESENTATION_CONTEXT(3)
GLOBAL_UNCERTAINTY_ASSIGNED_CONTEXT((#6588))
GLOBAL_UNIT_ASSIGNED_CONTEXT((#6639,#6641,#6642))
REPRESENTATION_CONTEXT('','3D')
);
#6618=(
GEOMETRIC_REPRESENTATION_CONTEXT(3)
GLOBAL_UNCERTAINTY_ASSIGNED_CONTEXT((#6589))
GLOBAL_UNIT_ASSIGNED_CONTEXT((#6639,#6641,#6642))
REPRESENTATION_CONTEXT('','3D')
);
#6619=(
GEOMETRIC_REPRESENTATION_CONTEXT(3)
GLOBAL_UNCERTAINTY_ASSIGNED_CONTEXT((#6590))
GLOBAL_UNIT_ASSIGNED_CONTEXT((#6639,#6641,#6642))
REPRESENTATION_CONTEXT('','3D')
);
#6620=(
GEOMETRIC_REPRESENTATION_CONTEXT(3)
GLOBAL_UNCERTAINTY_ASSIGNED_CONTEXT((#6591))
GLOBAL_UNIT_ASSIGNED_CONTEXT((#6639,#6641,#6642))
REPRESENTATION_CONTEXT('','3D')
);
#6621=(
GEOMETRIC_REPRESENTATION_CONTEXT(3)
GLOBAL_UNCERTAINTY_ASSIGNED_CONTEXT((#6592))
GLOBAL_UNIT_ASSIGNED_CONTEXT((#6639,#6641,#6642))
REPRESENTATION_CONTEXT('','3D')
);
#6622=(
GEOMETRIC_REPRESENTATION_CONTEXT(3)
GLOBAL_UNCERTAINTY_ASSIGNED_CONTEXT((#6593))
GLOBAL_UNIT_ASSIGNED_CONTEXT((#6639,#6641,#6642))
REPRESENTATION_CONTEXT('','3D')
);
#6623=(
GEOMETRIC_REPRESENTATION_CONTEXT(3)
GLOBAL_UNCERTAINTY_ASSIGNED_CONTEXT((#6594))
GLOBAL_UNIT_ASSIGNED_CONTEXT((#6639,#6641,#6642))
REPRESENTATION_CONTEXT('','3D')
);
#6624=(
GEOMETRIC_REPRESENTATION_CONTEXT(3)
GLOBAL_UNCERTAINTY_ASSIGNED_CONTEXT((#6595))
GLOBAL_UNIT_ASSIGNED_CONTEXT((#6639,#6641,#6642))
REPRESENTATION_CONTEXT('','3D')
);
#6625=(
GEOMETRIC_REPRESENTATION_CONTEXT(3)
GLOBAL_UNCERTAINTY_ASSIGNED_CONTEXT((#6596))
GLOBAL_UNIT_ASSIGNED_CONTEXT((#6639,#6641,#6642))
REPRESENTATION_CONTEXT('','3D')
);
#6626=(
GEOMETRIC_REPRESENTATION_CONTEXT(3)
GLOBAL_UNCERTAINTY_ASSIGNED_CONTEXT((#6597))
GLOBAL_UNIT_ASSIGNED_CONTEXT((#6639,#6641,#6642))
REPRESENTATION_CONTEXT('','3D')
);
#6627=(
GEOMETRIC_REPRESENTATION_CONTEXT(3)
GLOBAL_UNCERTAINTY_ASSIGNED_CONTEXT((#6598))
GLOBAL_UNIT_ASSIGNED_CONTEXT((#6639,#6641,#6642))
REPRESENTATION_CONTEXT('','3D')
);
#6628=(
GEOMETRIC_REPRESENTATION_CONTEXT(3)
GLOBAL_UNCERTAINTY_ASSIGNED_CONTEXT((#6599))
GLOBAL_UNIT_ASSIGNED_CONTEXT((#6639,#6641,#6642))
REPRESENTATION_CONTEXT('','3D')
);
#6629=(
GEOMETRIC_REPRESENTATION_CONTEXT(3)
GLOBAL_UNCERTAINTY_ASSIGNED_CONTEXT((#6600))
GLOBAL_UNIT_ASSIGNED_CONTEXT((#6639,#6641,#6642))
REPRESENTATION_CONTEXT('','3D')
);
#6630=(
GEOMETRIC_REPRESENTATION_CONTEXT(3)
GLOBAL_UNCERTAINTY_ASSIGNED_CONTEXT((#6601))
GLOBAL_UNIT_ASSIGNED_CONTEXT((#6639,#6641,#6642))
REPRESENTATION_CONTEXT('','3D')
);
#6631=(
GEOMETRIC_REPRESENTATION_CONTEXT(3)
GLOBAL_UNCERTAINTY_ASSIGNED_CONTEXT((#6602))
GLOBAL_UNIT_ASSIGNED_CONTEXT((#6639,#6641,#6642))
REPRESENTATION_CONTEXT('','3D')
);
#6632=(
GEOMETRIC_REPRESENTATION_CONTEXT(3)
GLOBAL_UNCERTAINTY_ASSIGNED_CONTEXT((#6603))
GLOBAL_UNIT_ASSIGNED_CONTEXT((#6639,#6641,#6642))
REPRESENTATION_CONTEXT('','3D')
);
#6633=(
GEOMETRIC_REPRESENTATION_CONTEXT(3)
GLOBAL_UNCERTAINTY_ASSIGNED_CONTEXT((#6604))
GLOBAL_UNIT_ASSIGNED_CONTEXT((#6639,#6641,#6642))
REPRESENTATION_CONTEXT('','3D')
);
#6634=(
GEOMETRIC_REPRESENTATION_CONTEXT(3)
GLOBAL_UNCERTAINTY_ASSIGNED_CONTEXT((#6605))
GLOBAL_UNIT_ASSIGNED_CONTEXT((#6639,#6641,#6642))
REPRESENTATION_CONTEXT('','3D')
);
#6635=(
GEOMETRIC_REPRESENTATION_CONTEXT(3)
GLOBAL_UNCERTAINTY_ASSIGNED_CONTEXT((#6606))
GLOBAL_UNIT_ASSIGNED_CONTEXT((#6639,#6641,#6642))
REPRESENTATION_CONTEXT('','3D')
);
#6636=(
GEOMETRIC_REPRESENTATION_CONTEXT(3)
GLOBAL_UNCERTAINTY_ASSIGNED_CONTEXT((#6607))
GLOBAL_UNIT_ASSIGNED_CONTEXT((#6639,#6641,#6642))
REPRESENTATION_CONTEXT('','3D')
);
#6637=(
GEOMETRIC_REPRESENTATION_CONTEXT(3)
GLOBAL_UNCERTAINTY_ASSIGNED_CONTEXT((#6608))
GLOBAL_UNIT_ASSIGNED_CONTEXT((#6639,#6641,#6642))
REPRESENTATION_CONTEXT('','3D')
);
#6638=(
GEOMETRIC_REPRESENTATION_CONTEXT(3)
GLOBAL_UNCERTAINTY_ASSIGNED_CONTEXT((#6609))
GLOBAL_UNIT_ASSIGNED_CONTEXT((#6639,#6641,#6642))
REPRESENTATION_CONTEXT('','3D')
);
#6639=(
LENGTH_UNIT()
NAMED_UNIT(*)
SI_UNIT(.CENTI.,.METRE.)
);
#6640=(
LENGTH_UNIT()
NAMED_UNIT(*)
SI_UNIT($,.METRE.)
);
#6641=(
NAMED_UNIT(*)
PLANE_ANGLE_UNIT()
SI_UNIT($,.RADIAN.)
);
#6642=(
NAMED_UNIT(*)
SI_UNIT($,.STERADIAN.)
SOLID_ANGLE_UNIT()
);
#6643=SHAPE_DEFINITION_REPRESENTATION(#6671,#6737);
#6644=SHAPE_DEFINITION_REPRESENTATION(#6672,#6738);
#6645=SHAPE_DEFINITION_REPRESENTATION(#6673,#6739);
#6646=SHAPE_DEFINITION_REPRESENTATION(#6674,#6740);
#6647=SHAPE_DEFINITION_REPRESENTATION(#6675,#6741);
#6648=SHAPE_DEFINITION_REPRESENTATION(#6676,#6742);
#6649=SHAPE_DEFINITION_REPRESENTATION(#6677,#6743);
#6650=SHAPE_DEFINITION_REPRESENTATION(#6678,#6744);
#6651=SHAPE_DEFINITION_REPRESENTATION(#6679,#6745);
#6652=SHAPE_DEFINITION_REPRESENTATION(#6680,#6746);
#6653=SHAPE_DEFINITION_REPRESENTATION(#6681,#6747);
#6654=SHAPE_DEFINITION_REPRESENTATION(#6682,#6748);
#6655=SHAPE_DEFINITION_REPRESENTATION(#6683,#6749);
#6656=SHAPE_DEFINITION_REPRESENTATION(#6684,#6750);
#6657=SHAPE_DEFINITION_REPRESENTATION(#6685,#6751);
#6658=SHAPE_DEFINITION_REPRESENTATION(#6686,#6752);
#6659=SHAPE_DEFINITION_REPRESENTATION(#6687,#6753);
#6660=SHAPE_DEFINITION_REPRESENTATION(#6688,#6754);
#6661=SHAPE_DEFINITION_REPRESENTATION(#6689,#6755);
#6662=SHAPE_DEFINITION_REPRESENTATION(#6718,#6756);
#6663=SHAPE_DEFINITION_REPRESENTATION(#6719,#6757);
#6664=SHAPE_DEFINITION_REPRESENTATION(#6720,#6758);
#6665=SHAPE_DEFINITION_REPRESENTATION(#6721,#6759);
#6666=SHAPE_DEFINITION_REPRESENTATION(#6722,#6760);
#6667=SHAPE_DEFINITION_REPRESENTATION(#6723,#6761);
#6668=SHAPE_DEFINITION_REPRESENTATION(#6729,#6762);
#6669=SHAPE_DEFINITION_REPRESENTATION(#6730,#6763);
#6670=SHAPE_DEFINITION_REPRESENTATION(#6731,#6764);
#6671=PRODUCT_DEFINITION_SHAPE('',$,#6766);
#6672=PRODUCT_DEFINITION_SHAPE('',$,#6767);
#6673=PRODUCT_DEFINITION_SHAPE('',$,#6768);
#6674=PRODUCT_DEFINITION_SHAPE('',$,#6769);
#6675=PRODUCT_DEFINITION_SHAPE('',$,#6770);
#6676=PRODUCT_DEFINITION_SHAPE('',$,#6771);
#6677=PRODUCT_DEFINITION_SHAPE('',$,#6772);
#6678=PRODUCT_DEFINITION_SHAPE('',$,#6773);
#6679=PRODUCT_DEFINITION_SHAPE('',$,#6774);
#6680=PRODUCT_DEFINITION_SHAPE('',$,#6775);
#6681=PRODUCT_DEFINITION_SHAPE('',$,#6776);
#6682=PRODUCT_DEFINITION_SHAPE('',$,#6777);
#6683=PRODUCT_DEFINITION_SHAPE('',$,#6778);
#6684=PRODUCT_DEFINITION_SHAPE('',$,#6779);
#6685=PRODUCT_DEFINITION_SHAPE('',$,#6780);
#6686=PRODUCT_DEFINITION_SHAPE('',$,#6781);
#6687=PRODUCT_DEFINITION_SHAPE('',$,#6782);
#6688=PRODUCT_DEFINITION_SHAPE('',$,#6783);
#6689=PRODUCT_DEFINITION_SHAPE('',$,#6784);
#6690=PRODUCT_DEFINITION_SHAPE($,$,#125);
#6691=PRODUCT_DEFINITION_SHAPE($,$,#126);
#6692=PRODUCT_DEFINITION_SHAPE($,$,#127);
#6693=PRODUCT_DEFINITION_SHAPE($,$,#128);
#6694=PRODUCT_DEFINITION_SHAPE($,$,#129);
#6695=PRODUCT_DEFINITION_SHAPE($,$,#130);
#6696=PRODUCT_DEFINITION_SHAPE($,$,#131);
#6697=PRODUCT_DEFINITION_SHAPE($,$,#132);
#6698=PRODUCT_DEFINITION_SHAPE($,$,#133);
#6699=PRODUCT_DEFINITION_SHAPE($,$,#134);
#6700=PRODUCT_DEFINITION_SHAPE($,$,#135);
#6701=PRODUCT_DEFINITION_SHAPE($,$,#136);
#6702=PRODUCT_DEFINITION_SHAPE($,$,#137);
#6703=PRODUCT_DEFINITION_SHAPE($,$,#138);
#6704=PRODUCT_DEFINITION_SHAPE($,$,#139);
#6705=PRODUCT_DEFINITION_SHAPE($,$,#140);
#6706=PRODUCT_DEFINITION_SHAPE($,$,#141);
#6707=PRODUCT_DEFINITION_SHAPE($,$,#142);
#6708=PRODUCT_DEFINITION_SHAPE($,$,#143);
#6709=PRODUCT_DEFINITION_SHAPE($,$,#144);
#6710=PRODUCT_DEFINITION_SHAPE($,$,#145);
#6711=PRODUCT_DEFINITION_SHAPE($,$,#146);
#6712=PRODUCT_DEFINITION_SHAPE($,$,#147);
#6713=PRODUCT_DEFINITION_SHAPE($,$,#148);
#6714=PRODUCT_DEFINITION_SHAPE($,$,#149);
#6715=PRODUCT_DEFINITION_SHAPE($,$,#150);
#6716=PRODUCT_DEFINITION_SHAPE($,$,#151);
#6717=PRODUCT_DEFINITION_SHAPE($,$,#152);
#6718=PRODUCT_DEFINITION_SHAPE('',$,#6785);
#6719=PRODUCT_DEFINITION_SHAPE('',$,#6786);
#6720=PRODUCT_DEFINITION_SHAPE('',$,#6787);
#6721=PRODUCT_DEFINITION_SHAPE('',$,#6788);
#6722=PRODUCT_DEFINITION_SHAPE('',$,#6789);
#6723=PRODUCT_DEFINITION_SHAPE('',$,#6790);
#6724=PRODUCT_DEFINITION_SHAPE($,$,#153);
#6725=PRODUCT_DEFINITION_SHAPE($,$,#154);
#6726=PRODUCT_DEFINITION_SHAPE($,$,#155);
#6727=PRODUCT_DEFINITION_SHAPE($,$,#156);
#6728=PRODUCT_DEFINITION_SHAPE($,$,#157);
#6729=PRODUCT_DEFINITION_SHAPE('',$,#6791);
#6730=PRODUCT_DEFINITION_SHAPE('',$,#6792);
#6731=PRODUCT_DEFINITION_SHAPE('',$,#6793);
#6732=PRODUCT_DEFINITION_SHAPE($,$,#158);
#6733=PRODUCT_DEFINITION_SHAPE($,$,#159);
#6734=PRODUCT_DEFINITION_SHAPE($,$,#160);
#6735=PRODUCT_DEFINITION_SHAPE($,$,#161);
#6736=PRODUCT_DEFINITION_SHAPE($,$,#162);
#6737=SHAPE_REPRESENTATION('',(#3881,#4326,#4327,#4328),#6610);
#6738=SHAPE_REPRESENTATION('',(#3882,#4179,#4180,#4181,#4182,#4183,#4184,
#4185,#4186,#4187,#4188,#4189,#4190,#4191,#4192,#4193,#4194,#4195,#4196,
#4197,#4198,#4199,#4200,#4201,#4202,#4203,#4204,#4205,#4206),#6611);
#6739=SHAPE_REPRESENTATION('',(#3883),#6612);
#6740=SHAPE_REPRESENTATION('',(#3932),#6613);
#6741=SHAPE_REPRESENTATION('',(#3938),#6614);
#6742=SHAPE_REPRESENTATION('',(#3944),#6615);
#6743=SHAPE_REPRESENTATION('',(#3950),#6616);
#6744=SHAPE_REPRESENTATION('',(#3956),#6617);
#6745=SHAPE_REPRESENTATION('',(#3996),#6618);
#6746=SHAPE_REPRESENTATION('',(#4003),#6619);
#6747=SHAPE_REPRESENTATION('',(#4025),#6620);
#6748=SHAPE_REPRESENTATION('',(#4047),#6621);
#6749=SHAPE_REPRESENTATION('',(#4061),#6622);
#6750=SHAPE_REPRESENTATION('',(#4070),#6623);
#6751=SHAPE_REPRESENTATION('',(#4079),#6624);
#6752=SHAPE_REPRESENTATION('',(#4113),#6625);
#6753=SHAPE_REPRESENTATION('',(#4122),#6626);
#6754=SHAPE_REPRESENTATION('',(#4131),#6627);
#6755=SHAPE_REPRESENTATION('',(#4155),#6628);
#6756=SHAPE_REPRESENTATION('',(#4207,#4296,#4297,#4298,#4299,#4300),#6629);
#6757=SHAPE_REPRESENTATION('',(#4208),#6630);
#6758=SHAPE_REPRESENTATION('',(#4244),#6631);
#6759=SHAPE_REPRESENTATION('',(#4257),#6632);
#6760=SHAPE_REPRESENTATION('',(#4270),#6633);
#6761=SHAPE_REPRESENTATION('',(#4283),#6634);
#6762=SHAPE_REPRESENTATION('',(#4301,#4324,#4325),#6635);
#6763=SHAPE_REPRESENTATION('',(#4302),#6636);
#6764=SHAPE_REPRESENTATION('',(#4318),#6637);
#6765=PRODUCT_DEFINITION_CONTEXT('part definition',#6851,'design');
#6766=PRODUCT_DEFINITION('PAT-032','PAT-032',#6794,
#6765);
#6767=PRODUCT_DEFINITION('Nest and frame','Nest and frame',#6795,#6765);
#6768=PRODUCT_DEFINITION('Base','Base',#6796,#6765);
#6769=PRODUCT_DEFINITION('Bonded foot','Bonded foot',#6797,#6765);
#6770=PRODUCT_DEFINITION('Bonded foot (1)','Bonded foot (1)',#6798,#6765);
#6771=PRODUCT_DEFINITION('Bonded foot (2)','Bonded foot (2)',#6799,#6765);
#6772=PRODUCT_DEFINITION('Bonded foot (3)','Bonded foot (3)',#6800,#6765);
#6773=PRODUCT_DEFINITION('Workpiece nest','Workpiece nest',#6801,#6765);
#6774=PRODUCT_DEFINITION('Example blank','Example blank',#6802,#6765);
#6775=PRODUCT_DEFINITION('Hinge lug','Hinge lug',#6803,#6765);
#6776=PRODUCT_DEFINITION('Hinge lug (1)','Hinge lug (1)',#6804,#6765);
#6777=PRODUCT_DEFINITION('Hinge pin','Hinge pin',#6805,#6765);
#6778=PRODUCT_DEFINITION('Pin keeper','Pin keeper',#6806,#6765);
#6779=PRODUCT_DEFINITION('Pin keeper (1)','Pin keeper (1)',#6807,#6765);
#6780=PRODUCT_DEFINITION('Latch post','Latch post',#6808,#6765);
#6781=PRODUCT_DEFINITION('Latch thrust spacer','Latch thrust spacer',#6809,
#6765);
#6782=PRODUCT_DEFINITION('Latch keeper','Latch keeper',#6810,#6765);
#6783=PRODUCT_DEFINITION('M5x14 Cap Screw','M5x14 Cap Screw',#6811,#6765);
#6784=PRODUCT_DEFINITION('M4x10 Cap Screw','M4x10 Cap Screw',#6812,#6765);
#6785=PRODUCT_DEFINITION('Hinged drill plate','Hinged drill plate',#6813,
#6765);
#6786=PRODUCT_DEFINITION('Bushing plate','Bushing plate',#6814,#6765);
#6787=PRODUCT_DEFINITION('Drill bushing 8','Drill bushing 8',#6815,#6765);
#6788=PRODUCT_DEFINITION('Drill bushing 8 (1)','Drill bushing 8 (1)',#6816,
#6765);
#6789=PRODUCT_DEFINITION('Drill bushing 10','Drill bushing 10',#6817,#6765);
#6790=PRODUCT_DEFINITION('Drill bushing 10 (1)','Drill bushing 10 (1)',#6818,
#6765);
#6791=PRODUCT_DEFINITION('Eccentric latch (1)','Eccentric latch (1)',#6819,
#6765);
#6792=PRODUCT_DEFINITION('Eccentric latch','Eccentric latch',#6820,#6765);
#6793=PRODUCT_DEFINITION('Bonded latch grip','Bonded latch grip',#6821,
#6765);
#6794=PRODUCT_DEFINITION_FORMATION('',$,#6853);
#6795=PRODUCT_DEFINITION_FORMATION('',$,#6854);
#6796=PRODUCT_DEFINITION_FORMATION('',$,#6855);
#6797=PRODUCT_DEFINITION_FORMATION('',$,#6856);
#6798=PRODUCT_DEFINITION_FORMATION('',$,#6857);
#6799=PRODUCT_DEFINITION_FORMATION('',$,#6858);
#6800=PRODUCT_DEFINITION_FORMATION('',$,#6859);
#6801=PRODUCT_DEFINITION_FORMATION('',$,#6860);
#6802=PRODUCT_DEFINITION_FORMATION('',$,#6861);
#6803=PRODUCT_DEFINITION_FORMATION('',$,#6862);
#6804=PRODUCT_DEFINITION_FORMATION('',$,#6863);
#6805=PRODUCT_DEFINITION_FORMATION('',$,#6864);
#6806=PRODUCT_DEFINITION_FORMATION('',$,#6865);
#6807=PRODUCT_DEFINITION_FORMATION('',$,#6866);
#6808=PRODUCT_DEFINITION_FORMATION('',$,#6867);
#6809=PRODUCT_DEFINITION_FORMATION('',$,#6868);
#6810=PRODUCT_DEFINITION_FORMATION('',$,#6869);
#6811=PRODUCT_DEFINITION_FORMATION('',$,#6870);
#6812=PRODUCT_DEFINITION_FORMATION('',$,#6871);
#6813=PRODUCT_DEFINITION_FORMATION('',$,#6872);
#6814=PRODUCT_DEFINITION_FORMATION('',$,#6873);
#6815=PRODUCT_DEFINITION_FORMATION('',$,#6874);
#6816=PRODUCT_DEFINITION_FORMATION('',$,#6875);
#6817=PRODUCT_DEFINITION_FORMATION('',$,#6876);
#6818=PRODUCT_DEFINITION_FORMATION('',$,#6877);
#6819=PRODUCT_DEFINITION_FORMATION('',$,#6878);
#6820=PRODUCT_DEFINITION_FORMATION('',$,#6879);
#6821=PRODUCT_DEFINITION_FORMATION('',$,#6880);
#6822=PRODUCT_RELATED_PRODUCT_CATEGORY('PAT-032','PAT-032',(#6853));
#6823=PRODUCT_RELATED_PRODUCT_CATEGORY('Nest and frame',
'Nest and frame',(#6854));
#6824=PRODUCT_RELATED_PRODUCT_CATEGORY('Base','Base',(#6855));
#6825=PRODUCT_RELATED_PRODUCT_CATEGORY('Bonded foot','Bonded foot',(#6856));
#6826=PRODUCT_RELATED_PRODUCT_CATEGORY('Bonded foot (1)',
'Bonded foot (1)',(#6857));
#6827=PRODUCT_RELATED_PRODUCT_CATEGORY('Bonded foot (2)',
'Bonded foot (2)',(#6858));
#6828=PRODUCT_RELATED_PRODUCT_CATEGORY('Bonded foot (3)',
'Bonded foot (3)',(#6859));
#6829=PRODUCT_RELATED_PRODUCT_CATEGORY('Workpiece nest',
'Workpiece nest',(#6860));
#6830=PRODUCT_RELATED_PRODUCT_CATEGORY('Example blank','Example blank',
(#6861));
#6831=PRODUCT_RELATED_PRODUCT_CATEGORY('Hinge lug','Hinge lug',(#6862));
#6832=PRODUCT_RELATED_PRODUCT_CATEGORY('Hinge lug (1)','Hinge lug (1)',
(#6863));
#6833=PRODUCT_RELATED_PRODUCT_CATEGORY('Hinge pin','Hinge pin',(#6864));
#6834=PRODUCT_RELATED_PRODUCT_CATEGORY('Pin keeper','Pin keeper',(#6865));
#6835=PRODUCT_RELATED_PRODUCT_CATEGORY('Pin keeper (1)',
'Pin keeper (1)',(#6866));
#6836=PRODUCT_RELATED_PRODUCT_CATEGORY('Latch post','Latch post',(#6867));
#6837=PRODUCT_RELATED_PRODUCT_CATEGORY('Latch thrust spacer',
'Latch thrust spacer',(#6868));
#6838=PRODUCT_RELATED_PRODUCT_CATEGORY('Latch keeper','Latch keeper',(#6869));
#6839=PRODUCT_RELATED_PRODUCT_CATEGORY('M5x14 Cap Screw',
'M5x14 Cap Screw',(#6870));
#6840=PRODUCT_RELATED_PRODUCT_CATEGORY('M4x10 Cap Screw',
'M4x10 Cap Screw',(#6871));
#6841=PRODUCT_RELATED_PRODUCT_CATEGORY('Hinged drill plate',
'Hinged drill plate',(#6872));
#6842=PRODUCT_RELATED_PRODUCT_CATEGORY('Bushing plate','Bushing plate',
(#6873));
#6843=PRODUCT_RELATED_PRODUCT_CATEGORY('Drill bushing 8',
'Drill bushing 8',(#6874));
#6844=PRODUCT_RELATED_PRODUCT_CATEGORY('Drill bushing 8 (1)',
'Drill bushing 8 (1)',(#6875));
#6845=PRODUCT_RELATED_PRODUCT_CATEGORY('Drill bushing 10',
'Drill bushing 10',(#6876));
#6846=PRODUCT_RELATED_PRODUCT_CATEGORY('Drill bushing 10 (1)',
'Drill bushing 10 (1)',(#6877));
#6847=PRODUCT_RELATED_PRODUCT_CATEGORY('Eccentric latch (1)',
'Eccentric latch (1)',(#6878));
#6848=PRODUCT_RELATED_PRODUCT_CATEGORY('Eccentric latch',
'Eccentric latch',(#6879));
#6849=PRODUCT_RELATED_PRODUCT_CATEGORY('Bonded latch grip',
'Bonded latch grip',(#6880));
#6850=APPLICATION_PROTOCOL_DEFINITION('international standard',
'automotive_design',2009,#6851);
#6851=APPLICATION_CONTEXT(
'Core Data for Automotive Mechanical Design Process');
#6852=PRODUCT_CONTEXT('part definition',#6851,'mechanical');
#6853=PRODUCT('PAT-032','PAT-032',
'PAT-032',(#6852));
#6854=PRODUCT('Nest and frame','Nest and frame','Nest and frame',(#6852));
#6855=PRODUCT('Base','Base','Base',(#6852));
#6856=PRODUCT('Bonded foot','Bonded foot','Bonded foot',(#6852));
#6857=PRODUCT('Bonded foot (1)','Bonded foot (1)','Bonded foot (1)',(#6852));
#6858=PRODUCT('Bonded foot (2)','Bonded foot (2)','Bonded foot (2)',(#6852));
#6859=PRODUCT('Bonded foot (3)','Bonded foot (3)','Bonded foot (3)',(#6852));
#6860=PRODUCT('Workpiece nest','Workpiece nest','Workpiece nest',(#6852));
#6861=PRODUCT('Example blank','Example blank','Example blank',(#6852));
#6862=PRODUCT('Hinge lug','Hinge lug','Hinge lug',(#6852));
#6863=PRODUCT('Hinge lug (1)','Hinge lug (1)','Hinge lug (1)',(#6852));
#6864=PRODUCT('Hinge pin','Hinge pin','Hinge pin',(#6852));
#6865=PRODUCT('Pin keeper','Pin keeper','Pin keeper',(#6852));
#6866=PRODUCT('Pin keeper (1)','Pin keeper (1)','Pin keeper (1)',(#6852));
#6867=PRODUCT('Latch post','Latch post','Latch post',(#6852));
#6868=PRODUCT('Latch thrust spacer','Latch thrust spacer',
'Latch thrust spacer',(#6852));
#6869=PRODUCT('Latch keeper','Latch keeper','Latch keeper',(#6852));
#6870=PRODUCT('M5x14 Cap Screw','M5x14 Cap Screw','M5x14 Cap Screw',(#6852));
#6871=PRODUCT('M4x10 Cap Screw','M4x10 Cap Screw','M4x10 Cap Screw',(#6852));
#6872=PRODUCT('Hinged drill plate','Hinged drill plate',
'Hinged drill plate',(#6852));
#6873=PRODUCT('Bushing plate','Bushing plate','Bushing plate',(#6852));
#6874=PRODUCT('Drill bushing 8','Drill bushing 8','Drill bushing 8',(#6852));
#6875=PRODUCT('Drill bushing 8 (1)','Drill bushing 8 (1)',
'Drill bushing 8 (1)',(#6852));
#6876=PRODUCT('Drill bushing 10','Drill bushing 10','Drill bushing 10',
(#6852));
#6877=PRODUCT('Drill bushing 10 (1)','Drill bushing 10 (1)',
'Drill bushing 10 (1)',(#6852));
#6878=PRODUCT('Eccentric latch (1)','Eccentric latch (1)','Eccentric latch (1)',
(#6852));
#6879=PRODUCT('Eccentric latch','Eccentric latch','Eccentric latch',(#6852));
#6880=PRODUCT('Bonded latch grip','Bonded latch grip',
'Bonded latch grip',(#6852));
#6881=PRESENTATION_STYLE_ASSIGNMENT((#6886));
#6882=PRESENTATION_STYLE_ASSIGNMENT((#6887));
#6883=PRESENTATION_STYLE_ASSIGNMENT((#6888));
#6884=PRESENTATION_STYLE_ASSIGNMENT((#6889));
#6885=PRESENTATION_STYLE_ASSIGNMENT((#6890));
#6886=SURFACE_STYLE_USAGE(.BOTH.,#6891);
#6887=SURFACE_STYLE_USAGE(.BOTH.,#6892);
#6888=SURFACE_STYLE_USAGE(.BOTH.,#6893);
#6889=SURFACE_STYLE_USAGE(.BOTH.,#6894);
#6890=SURFACE_STYLE_USAGE(.BOTH.,#6895);
#6891=SURFACE_SIDE_STYLE('',(#6896));
#6892=SURFACE_SIDE_STYLE('',(#6897));
#6893=SURFACE_SIDE_STYLE('',(#6898));
#6894=SURFACE_SIDE_STYLE('',(#6899));
#6895=SURFACE_SIDE_STYLE('',(#6900));
#6896=SURFACE_STYLE_FILL_AREA(#6901);
#6897=SURFACE_STYLE_FILL_AREA(#6902);
#6898=SURFACE_STYLE_FILL_AREA(#6903);
#6899=SURFACE_STYLE_FILL_AREA(#6904);
#6900=SURFACE_STYLE_FILL_AREA(#6905);
#6901=FILL_AREA_STYLE('Steel - Satin',(#6906));
#6902=FILL_AREA_STYLE('CAD Library Painted - Deep blue',(#6907));
#6903=FILL_AREA_STYLE('CAD Library Painted - Engineering blue',(#6908));
#6904=FILL_AREA_STYLE('CAD Library Painted - Steel gray',(#6909));
#6905=FILL_AREA_STYLE('CAD Library Painted - Graphite',(#6910));
#6906=FILL_AREA_STYLE_COLOUR('Steel - Satin',#6911);
#6907=FILL_AREA_STYLE_COLOUR('CAD Library Painted - Deep blue',#6912);
#6908=FILL_AREA_STYLE_COLOUR('CAD Library Painted - Engineering blue',#6913);
#6909=FILL_AREA_STYLE_COLOUR('CAD Library Painted - Steel gray',#6914);
#6910=FILL_AREA_STYLE_COLOUR('CAD Library Painted - Graphite',#6915);
#6911=COLOUR_RGB('Steel - Satin',0.627450980392157,0.627450980392157,0.627450980392157);
#6912=COLOUR_RGB('CAD Library Painted - Deep blue',0.0784313725490196,0.203921568627451,
0.349019607843137);
#6913=COLOUR_RGB('CAD Library Painted - Engineering blue',0.12156862745098,
0.356862745098039,0.6);
#6914=COLOUR_RGB('CAD Library Painted - Steel gray',0.592156862745098,0.631372549019608,
0.67843137254902);
#6915=COLOUR_RGB('CAD Library Painted - Graphite',0.168627450980392,0.192156862745098,
0.231372549019608);
#6916=COLOUR_RGB('Dark Blue',0.08,0.2,0.34);
#6917=FILL_AREA_STYLE_COLOUR('',#6916);
#6918=FILL_AREA_STYLE('',(#6917));
#6919=SURFACE_STYLE_FILL_AREA(#6918);
#6920=SURFACE_SIDE_STYLE('',(#6919));
#6921=SURFACE_STYLE_USAGE(.BOTH.,#6920);
#6922=PRESENTATION_STYLE_ASSIGNMENT((#6921));
#6923=COLOUR_RGB('Light Blue',0.38,0.62,0.78);
#6924=FILL_AREA_STYLE_COLOUR('',#6923);
#6925=FILL_AREA_STYLE('',(#6924));
#6926=SURFACE_STYLE_FILL_AREA(#6925);
#6927=SURFACE_SIDE_STYLE('',(#6926));
#6928=SURFACE_STYLE_USAGE(.BOTH.,#6927);
#6929=PRESENTATION_STYLE_ASSIGNMENT((#6928));
#6930=COLOUR_RGB('Sky Blue',0.24,0.69,0.87);
#6931=FILL_AREA_STYLE_COLOUR('',#6930);
#6932=FILL_AREA_STYLE('',(#6931));
#6933=SURFACE_STYLE_FILL_AREA(#6932);
#6934=SURFACE_SIDE_STYLE('',(#6933));
#6935=SURFACE_STYLE_USAGE(.BOTH.,#6934);
#6936=PRESENTATION_STYLE_ASSIGNMENT((#6935));
#6937=COLOUR_RGB('Grey',0.48,0.52,0.57);
#6938=FILL_AREA_STYLE_COLOUR('',#6937);
#6939=FILL_AREA_STYLE('',(#6938));
#6940=SURFACE_STYLE_FILL_AREA(#6939);
#6941=SURFACE_SIDE_STYLE('',(#6940));
#6942=SURFACE_STYLE_USAGE(.BOTH.,#6941);
#6943=PRESENTATION_STYLE_ASSIGNMENT((#6942));
#6944=COLOUR_RGB('Black',0.12,0.14,0.17);
#6945=FILL_AREA_STYLE_COLOUR('',#6944);
#6946=FILL_AREA_STYLE('',(#6945));
#6947=SURFACE_STYLE_FILL_AREA(#6946);
#6948=SURFACE_SIDE_STYLE('',(#6947));
#6949=SURFACE_STYLE_USAGE(.BOTH.,#6948);
#6950=PRESENTATION_STYLE_ASSIGNMENT((#6949));
#6951=COLOUR_RGB('Off White',0.89,0.88,0.83);
#6952=FILL_AREA_STYLE_COLOUR('',#6951);
#6953=FILL_AREA_STYLE('',(#6952));
#6954=SURFACE_STYLE_FILL_AREA(#6953);
#6955=SURFACE_SIDE_STYLE('',(#6954));
#6956=SURFACE_STYLE_USAGE(.BOTH.,#6955);
#6957=PRESENTATION_STYLE_ASSIGNMENT((#6956));
ENDSEC;
END-ISO-10303-21;
